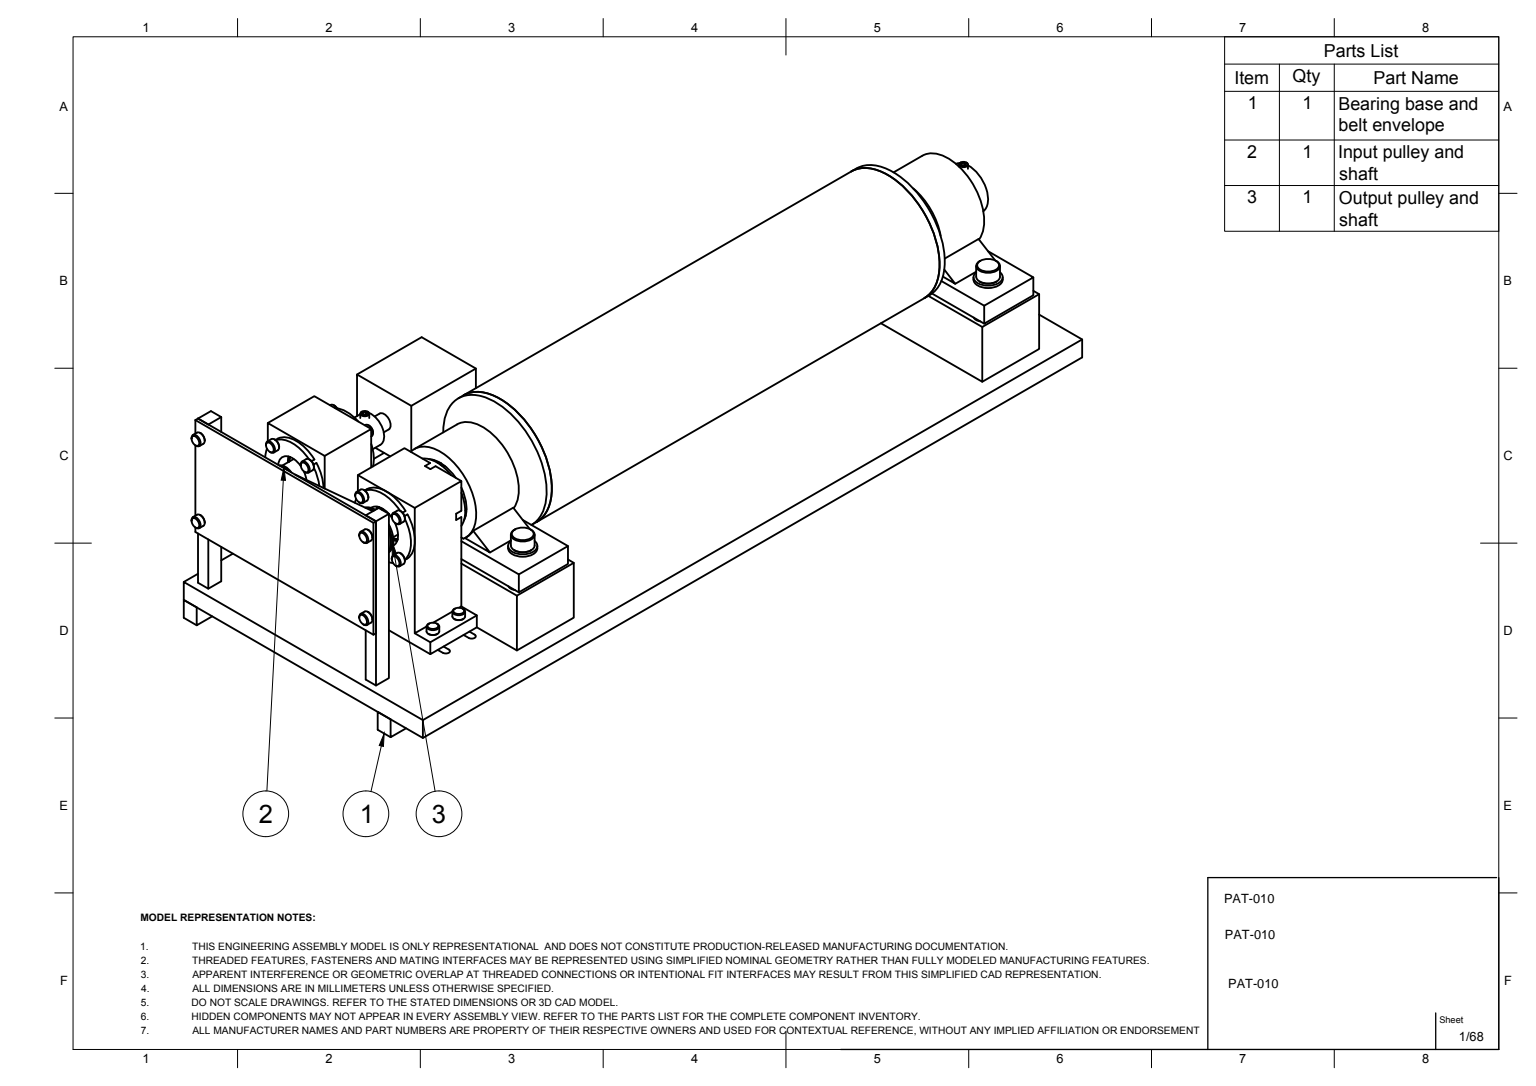
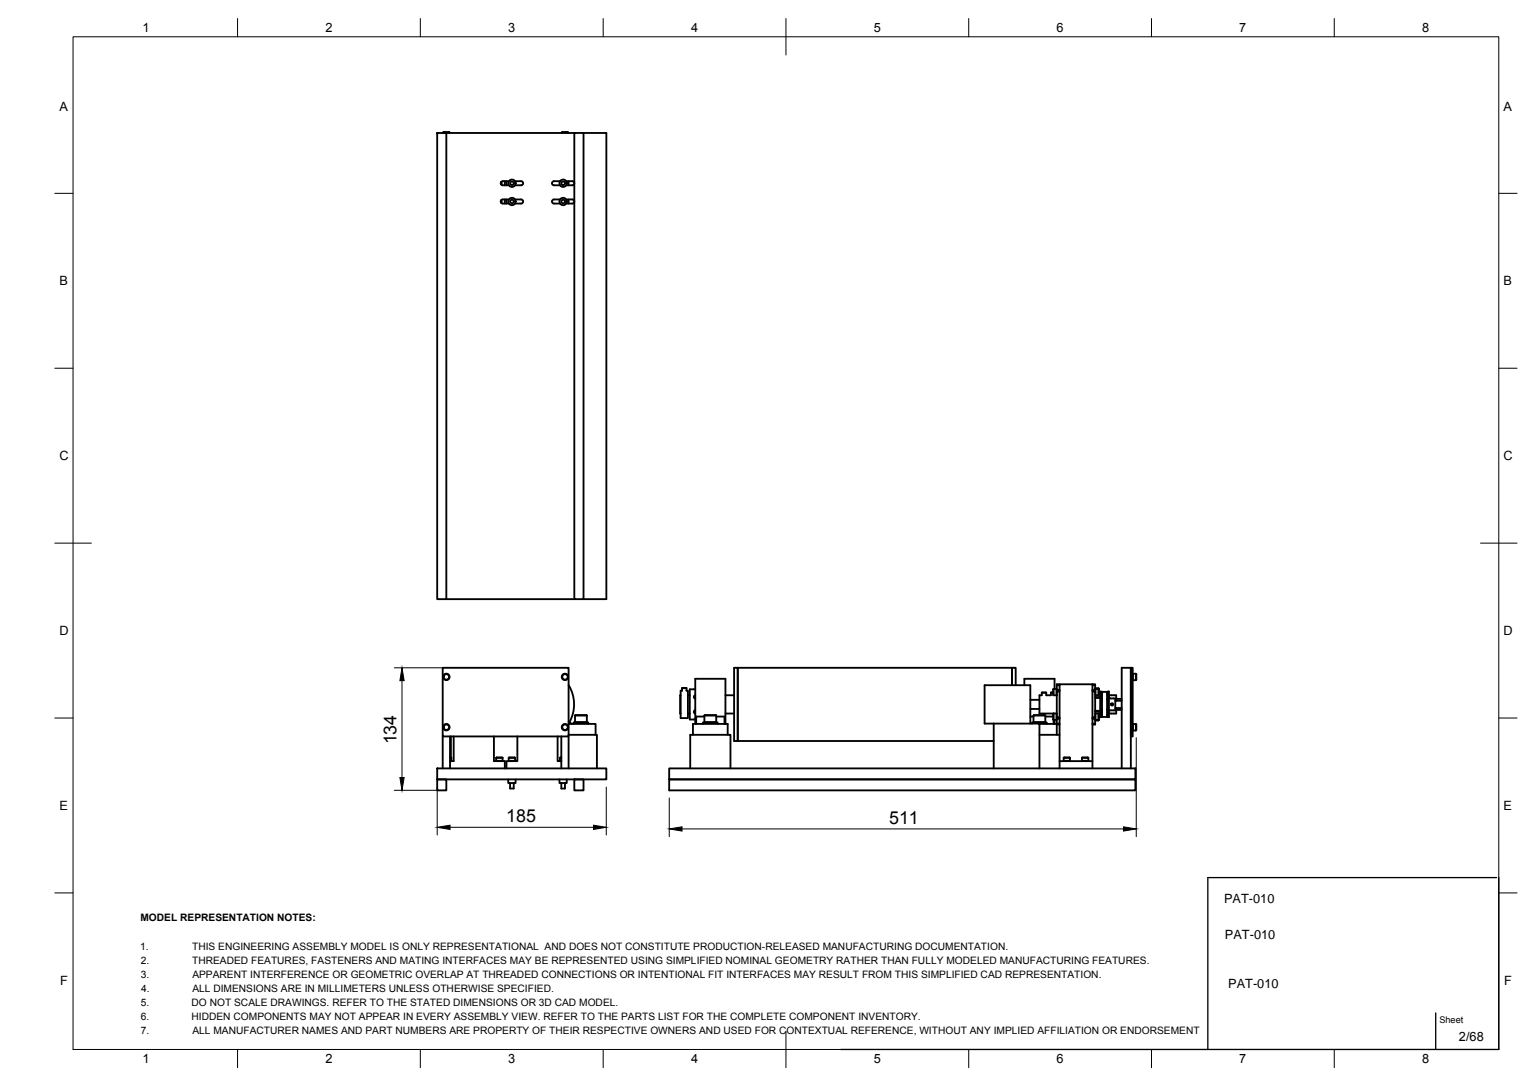
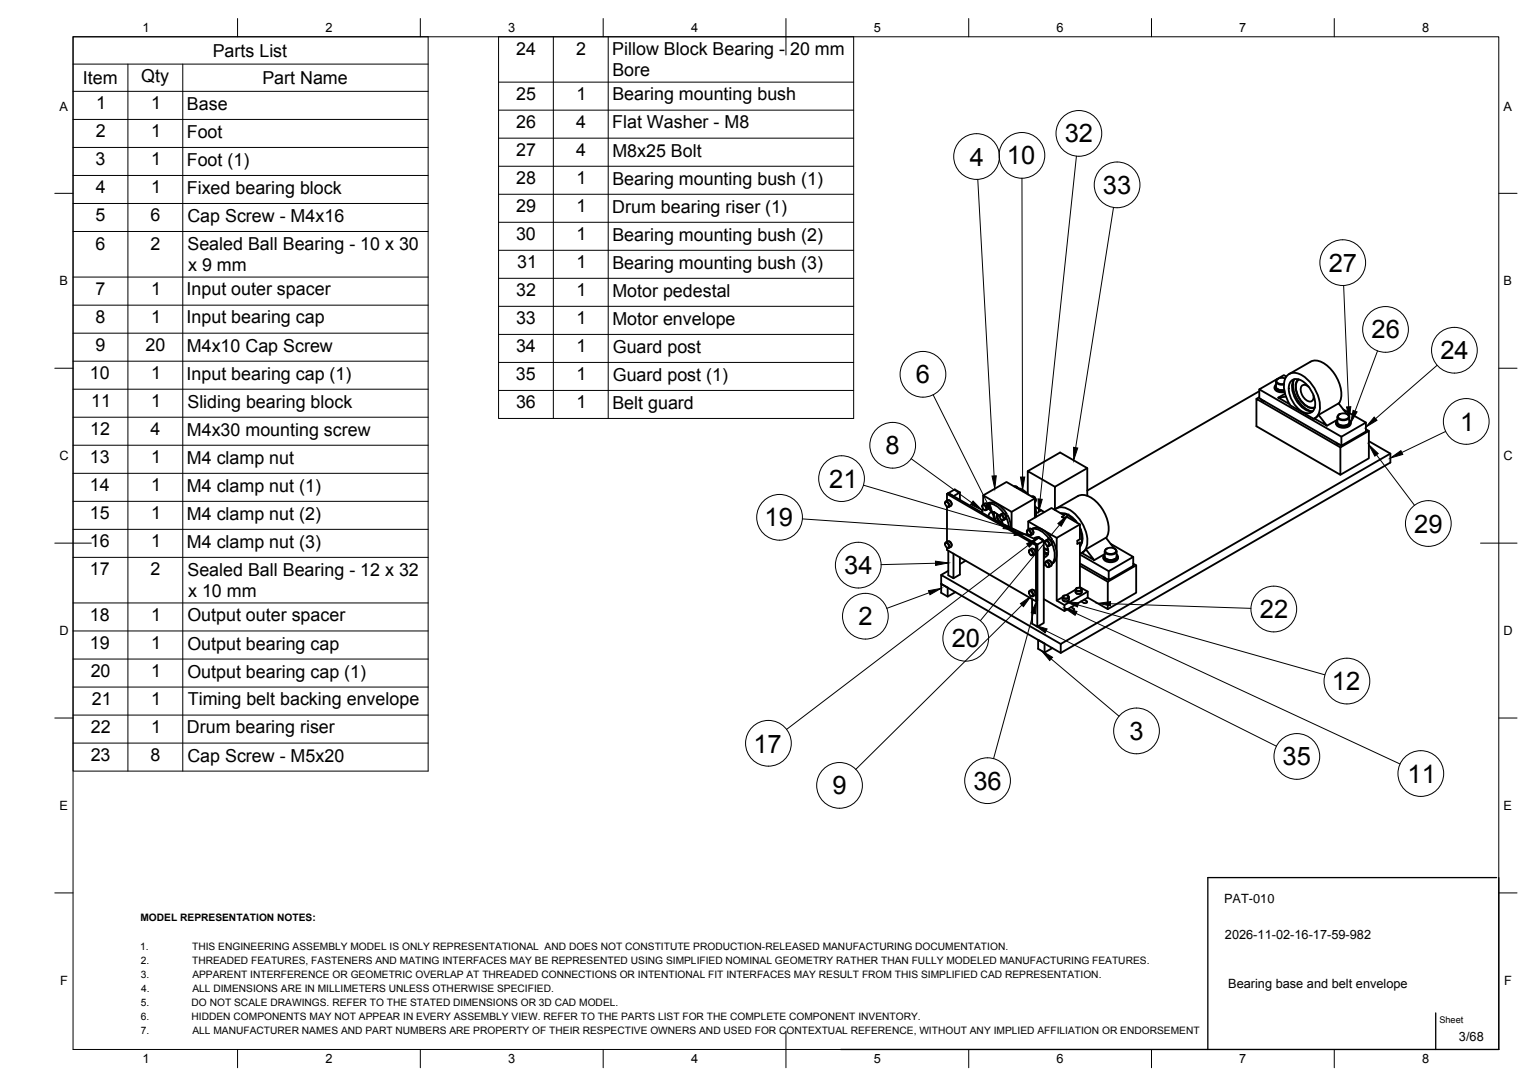
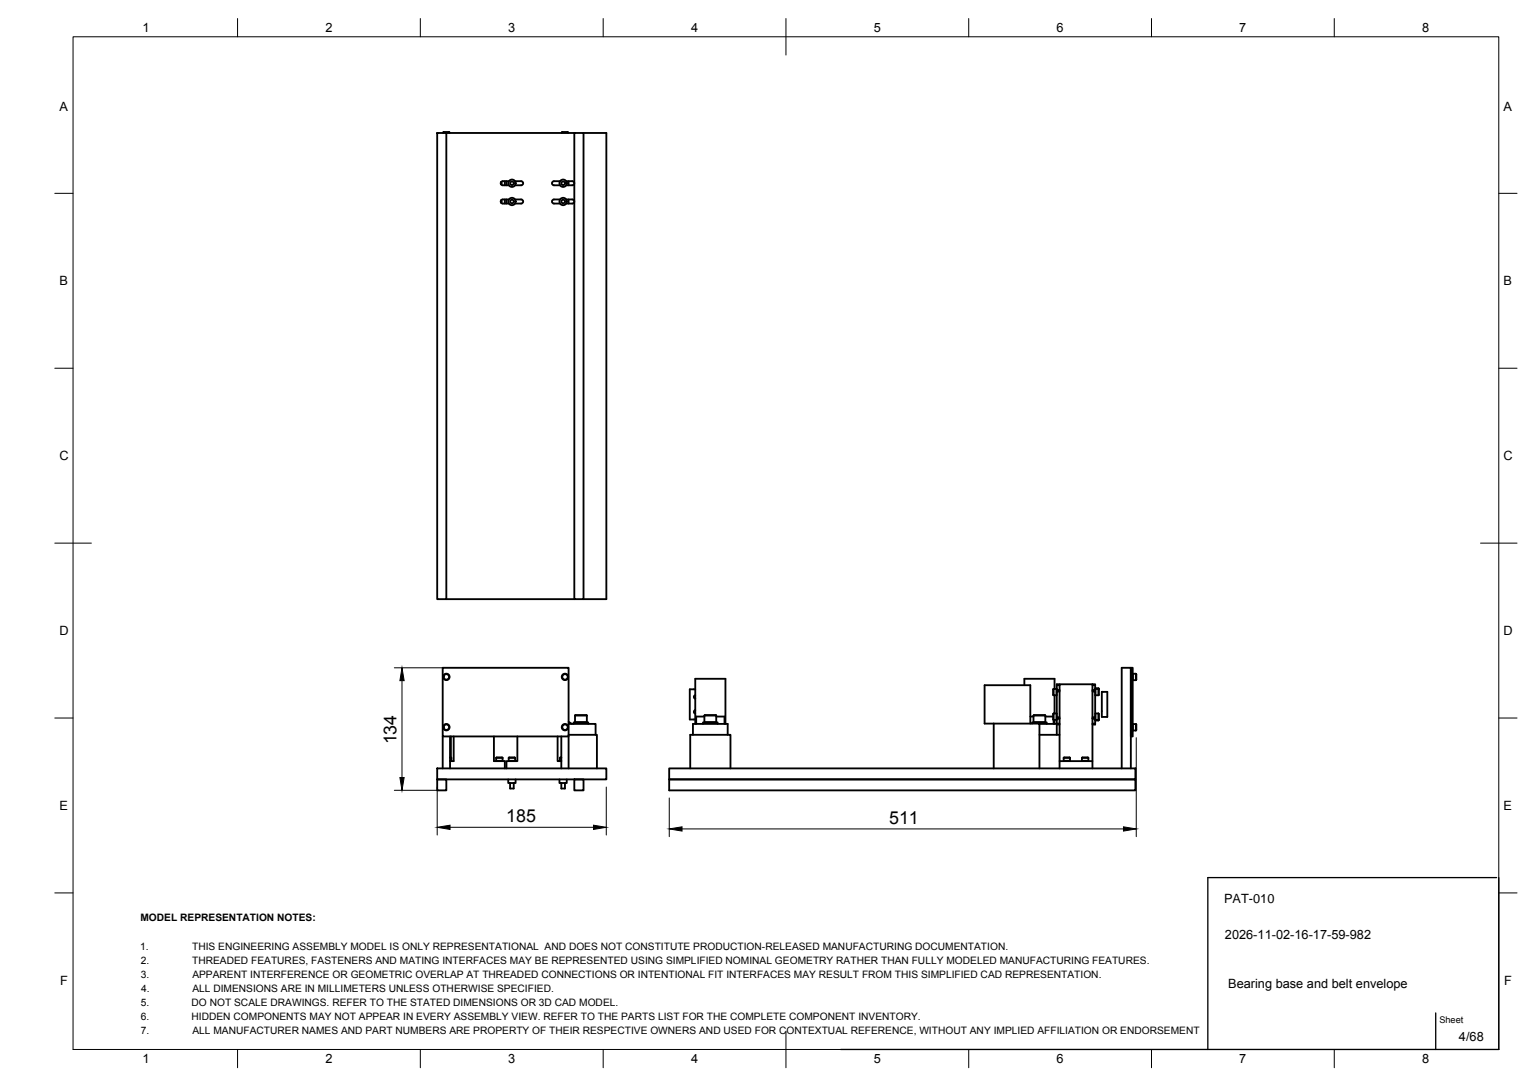
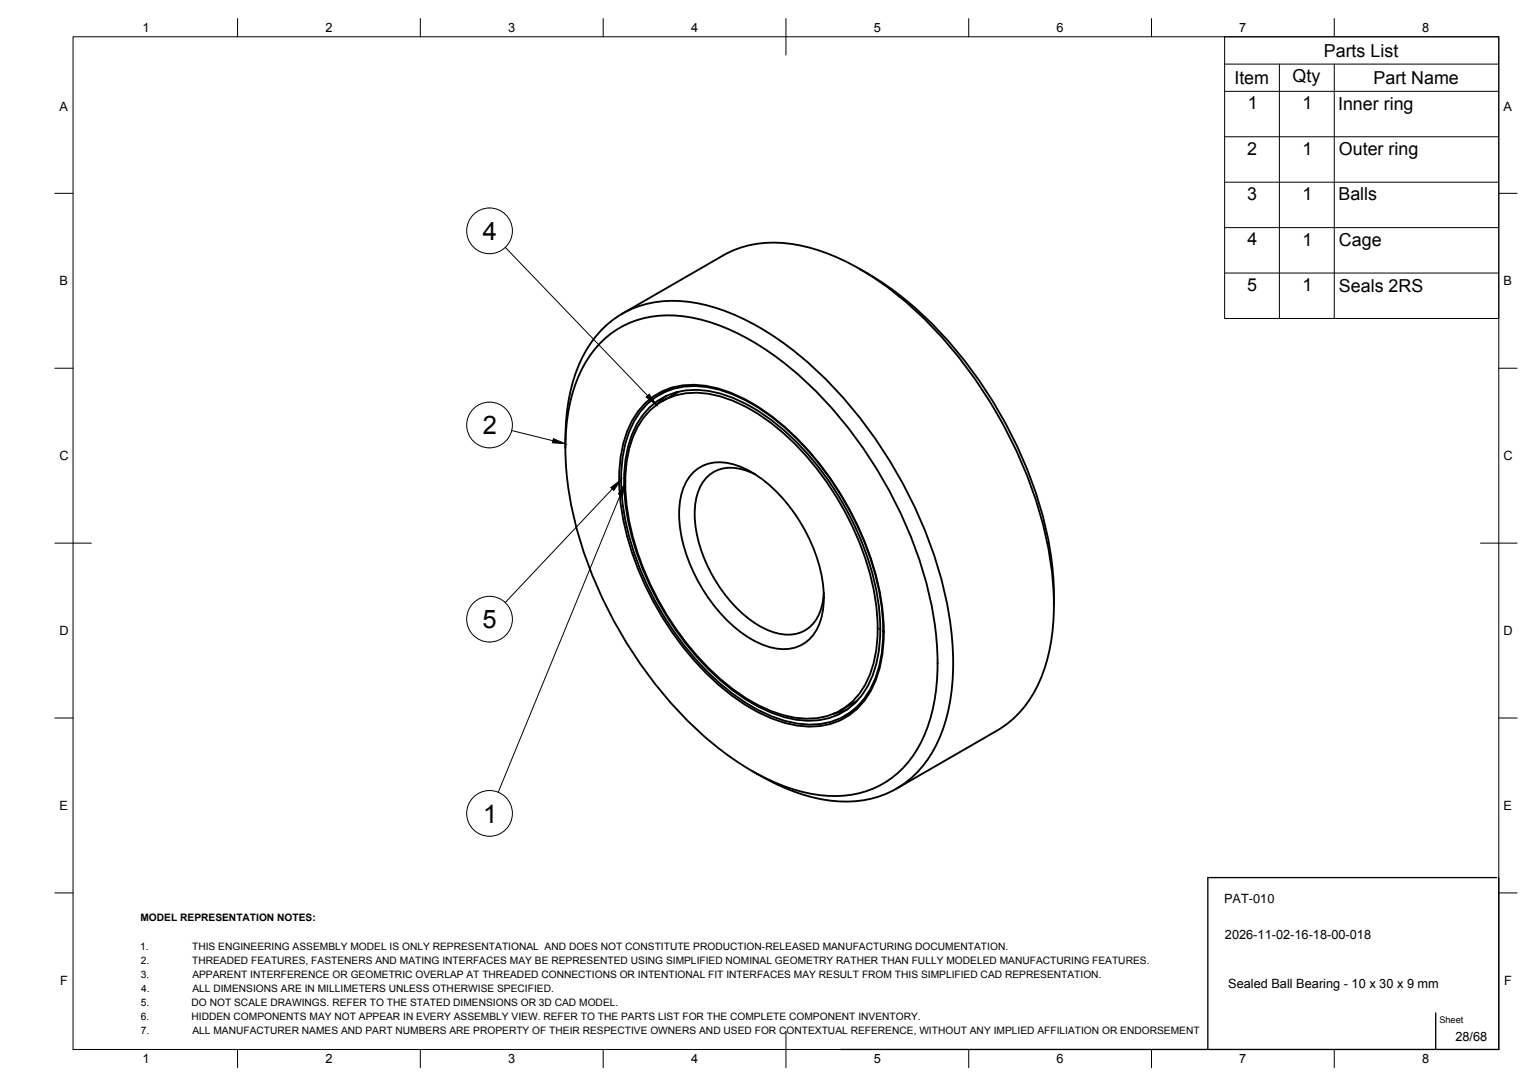
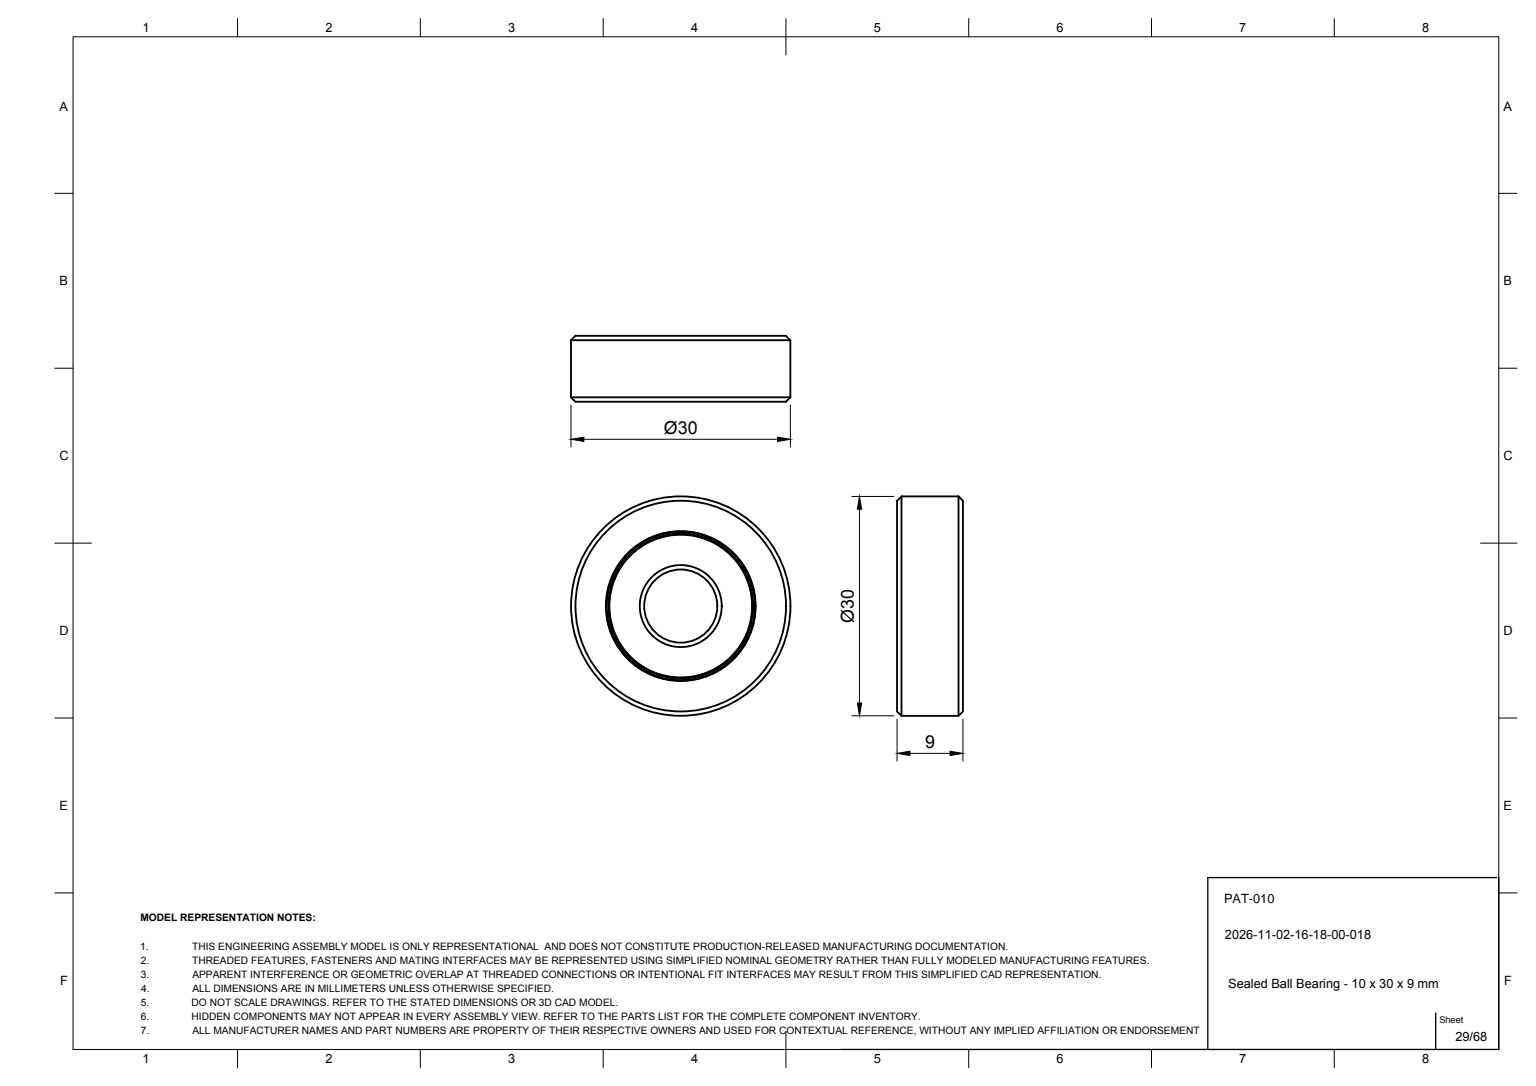
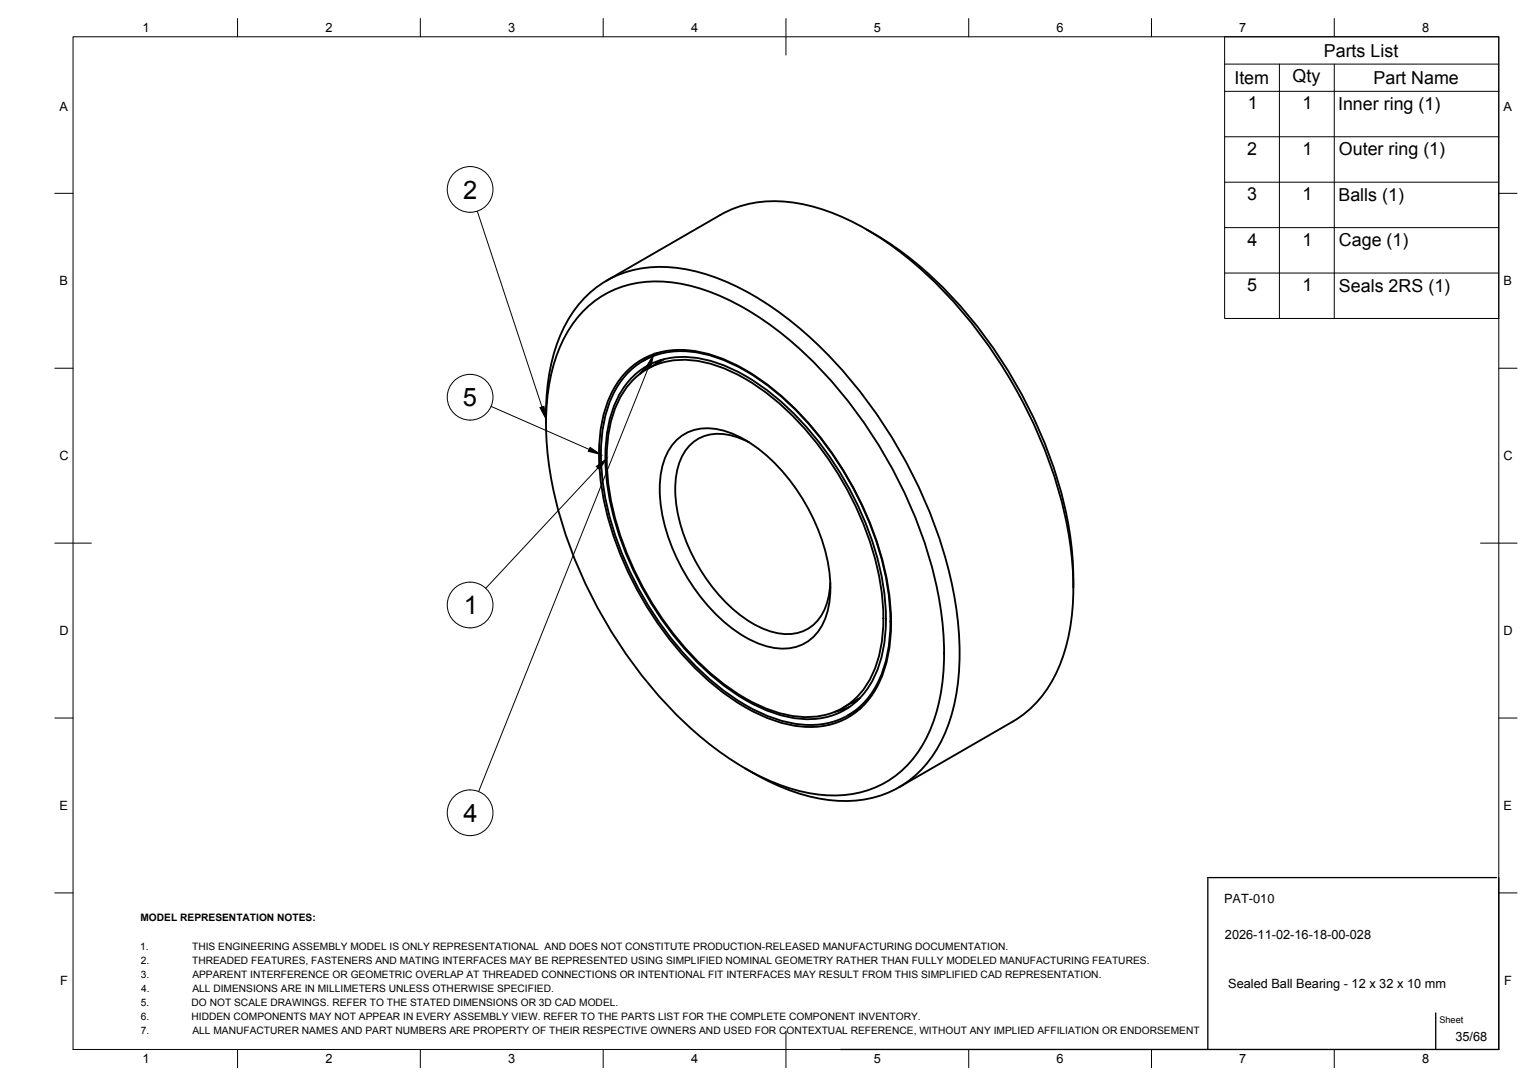
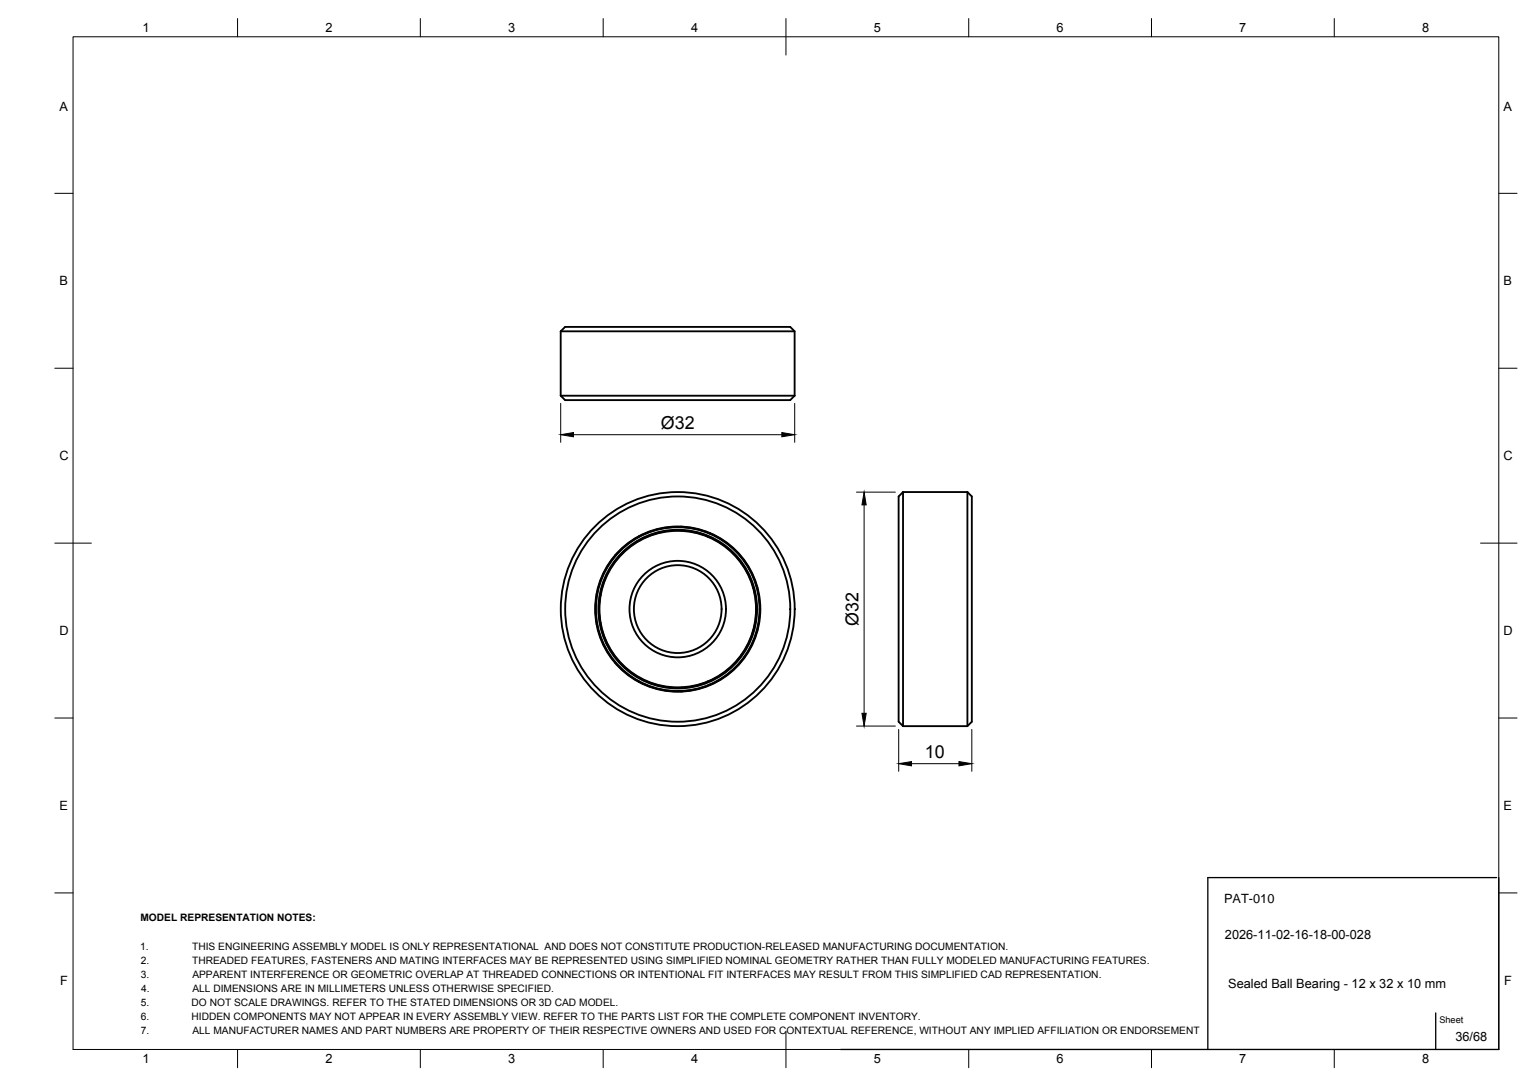
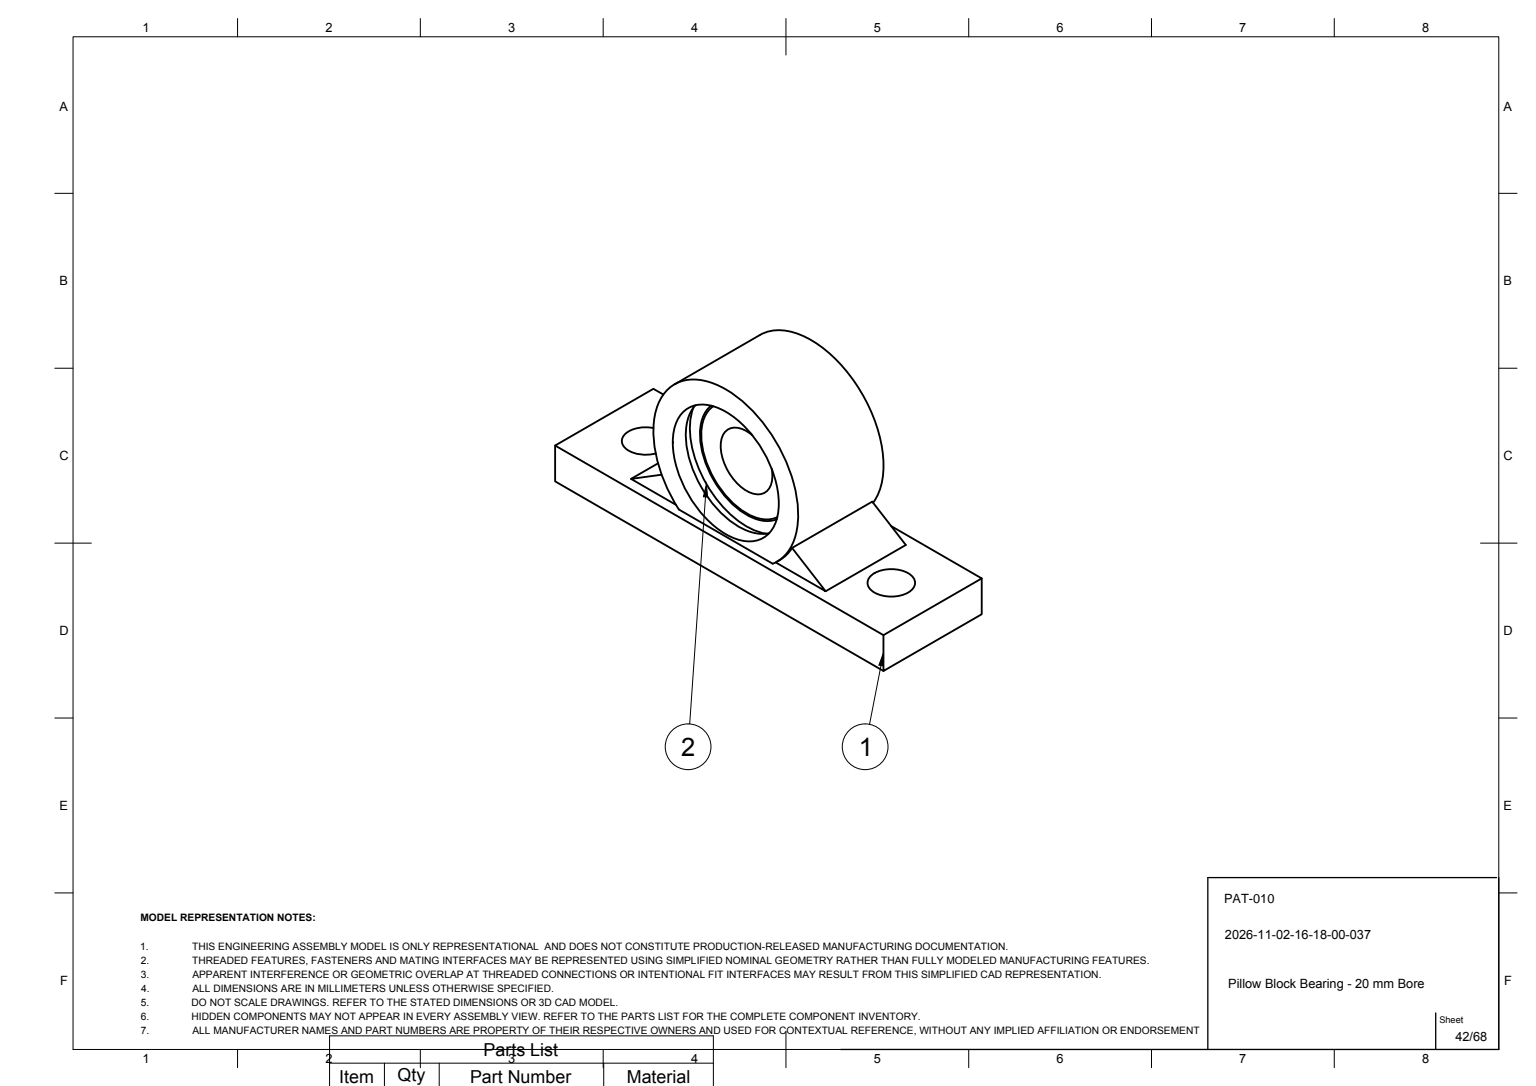
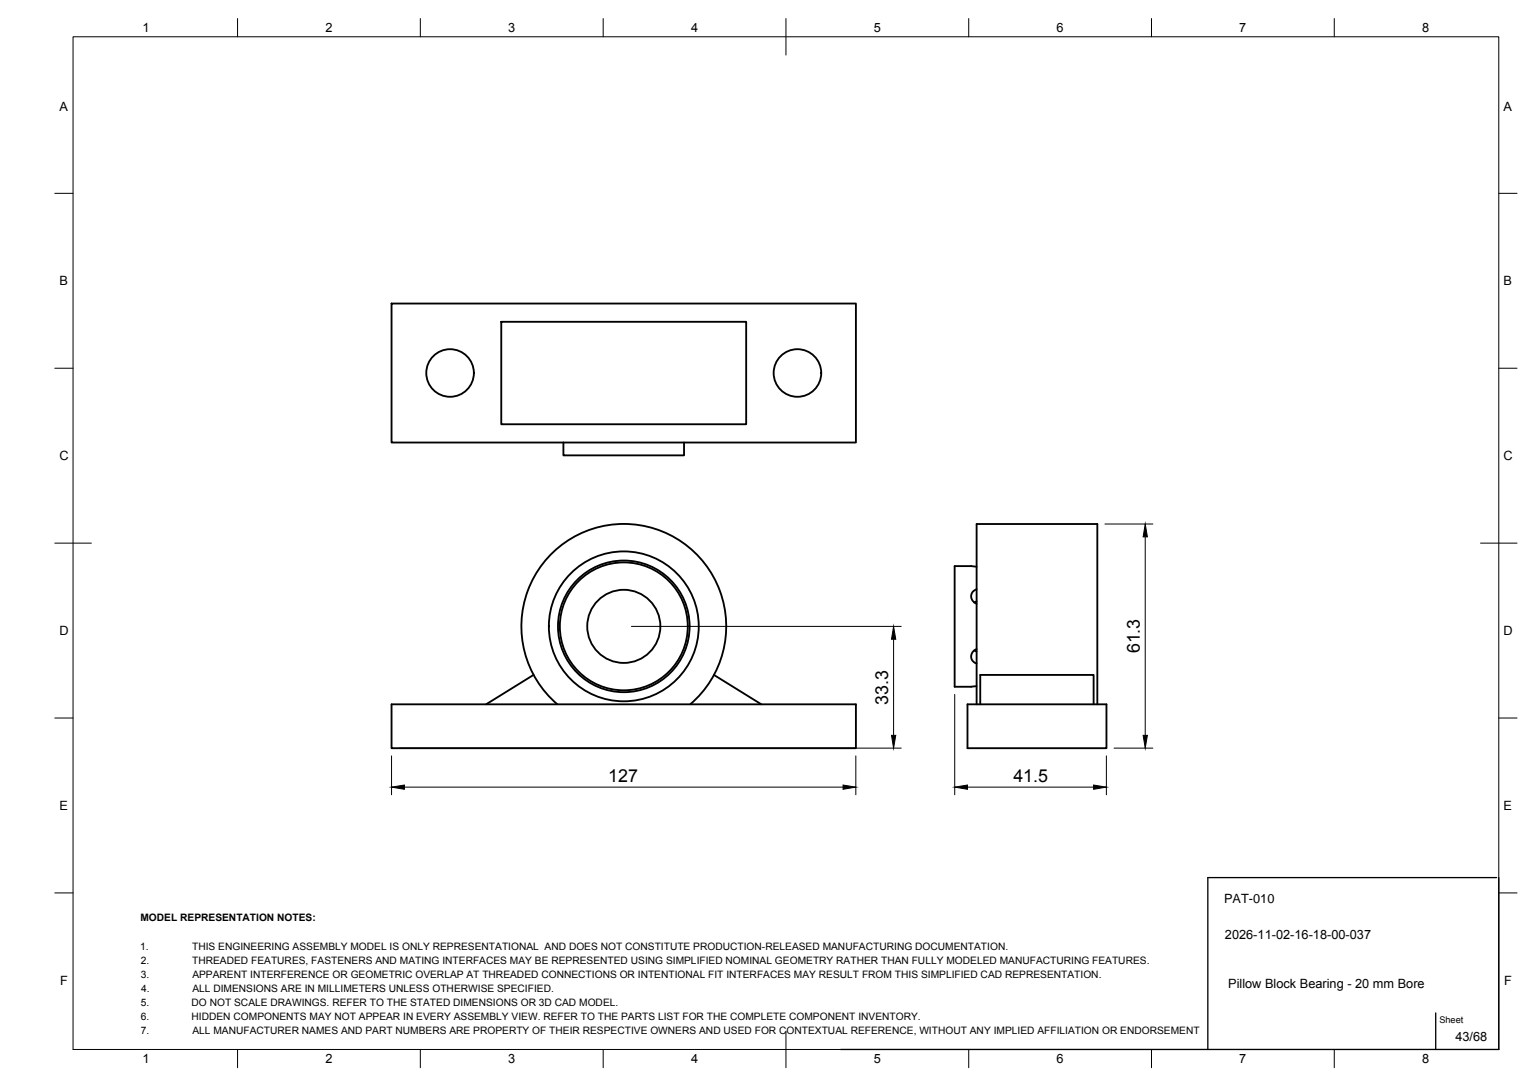
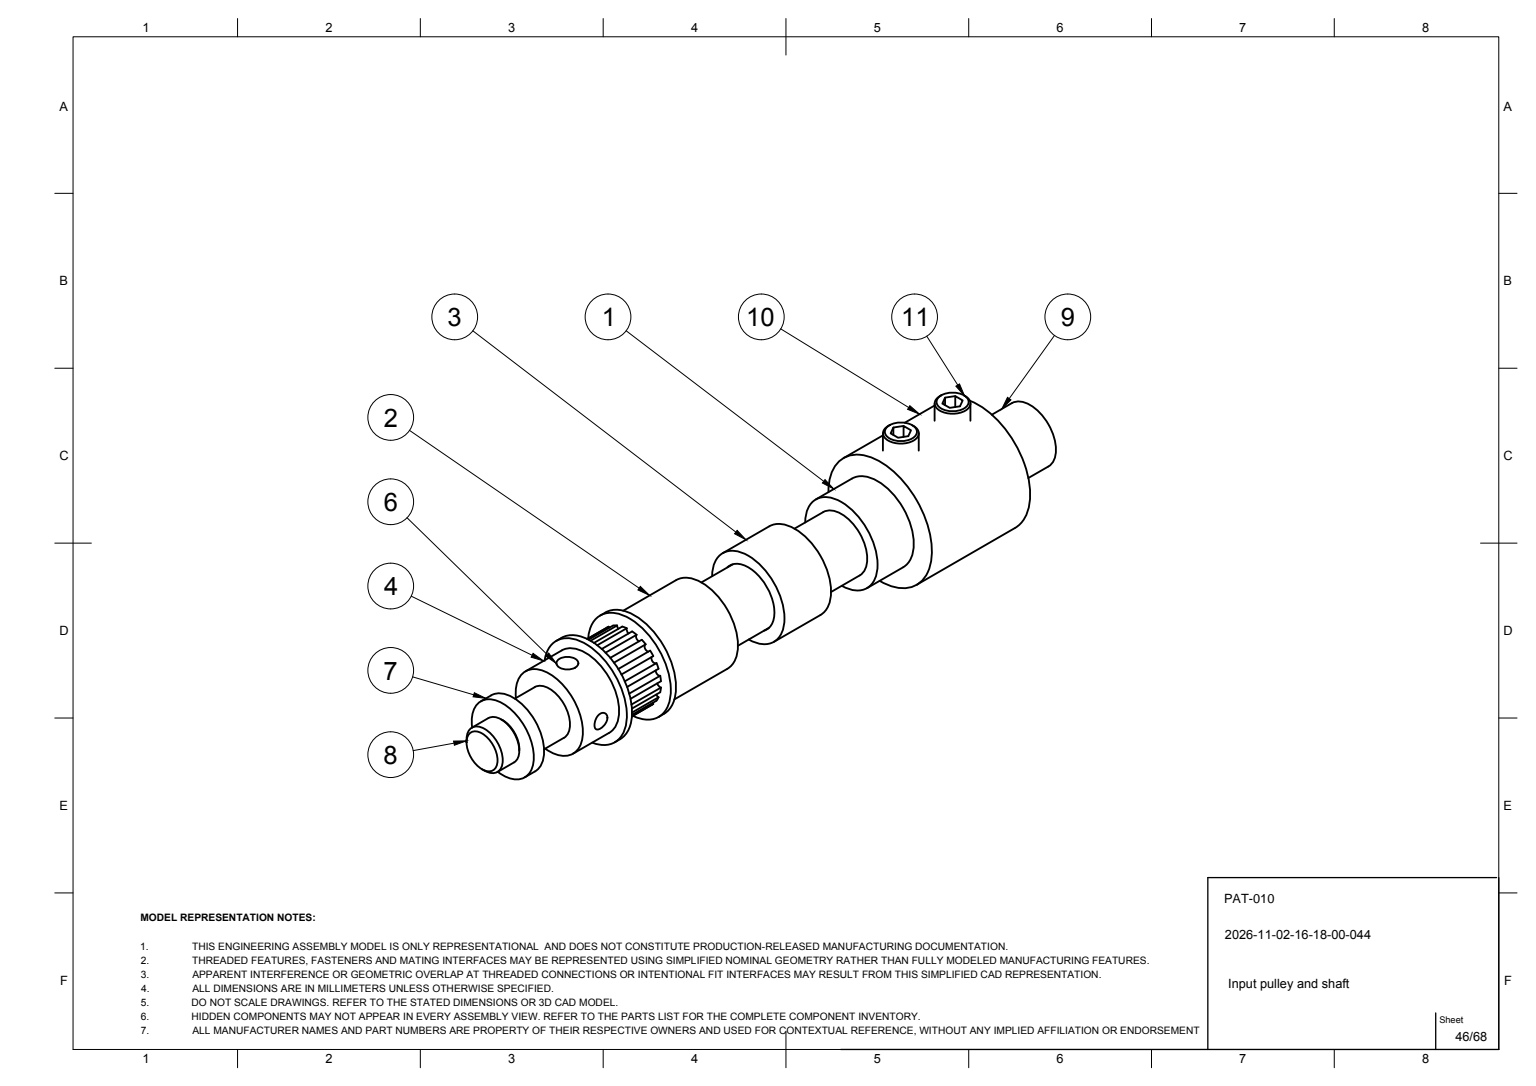
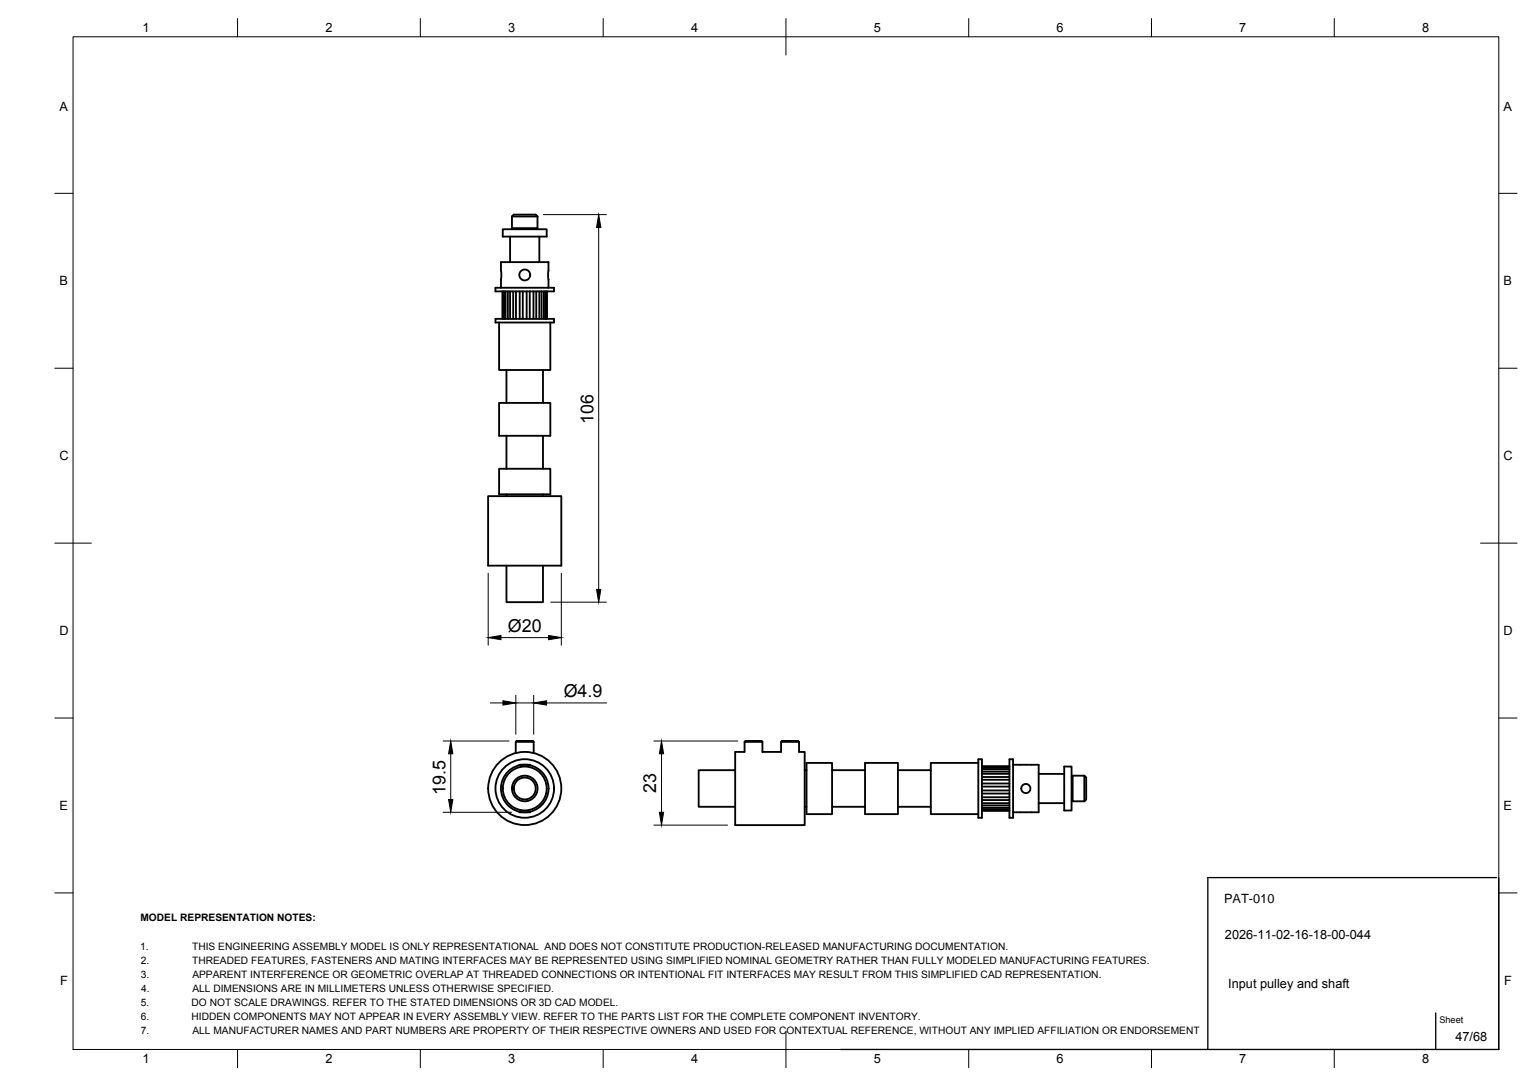
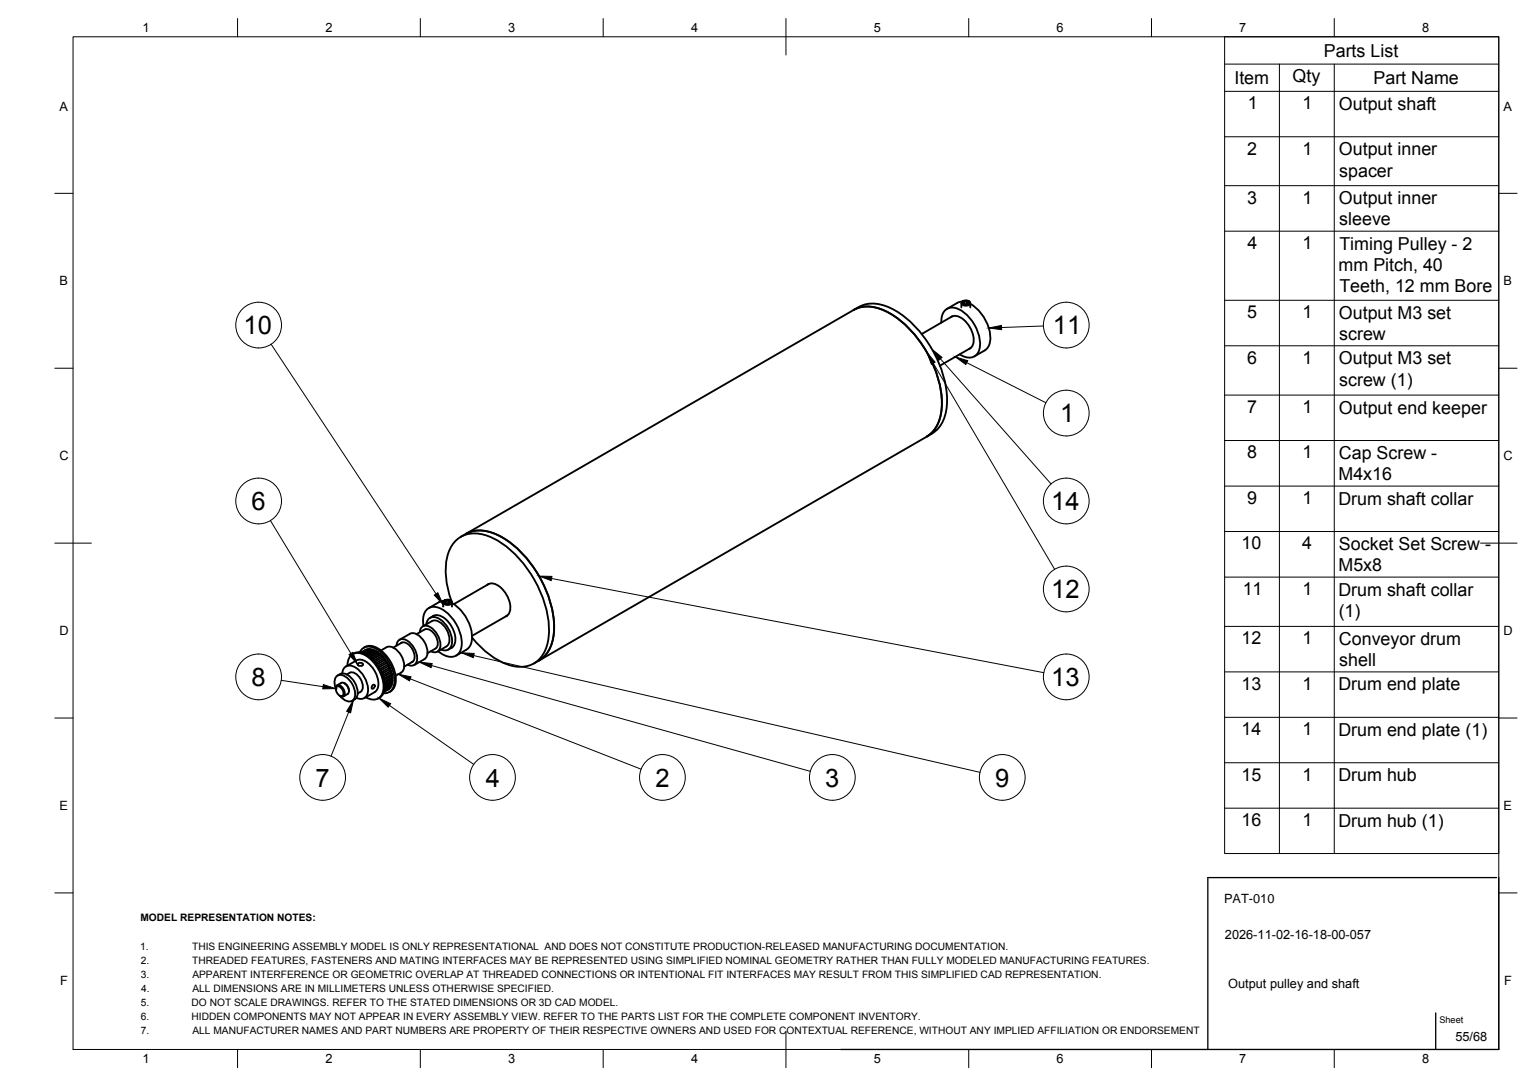
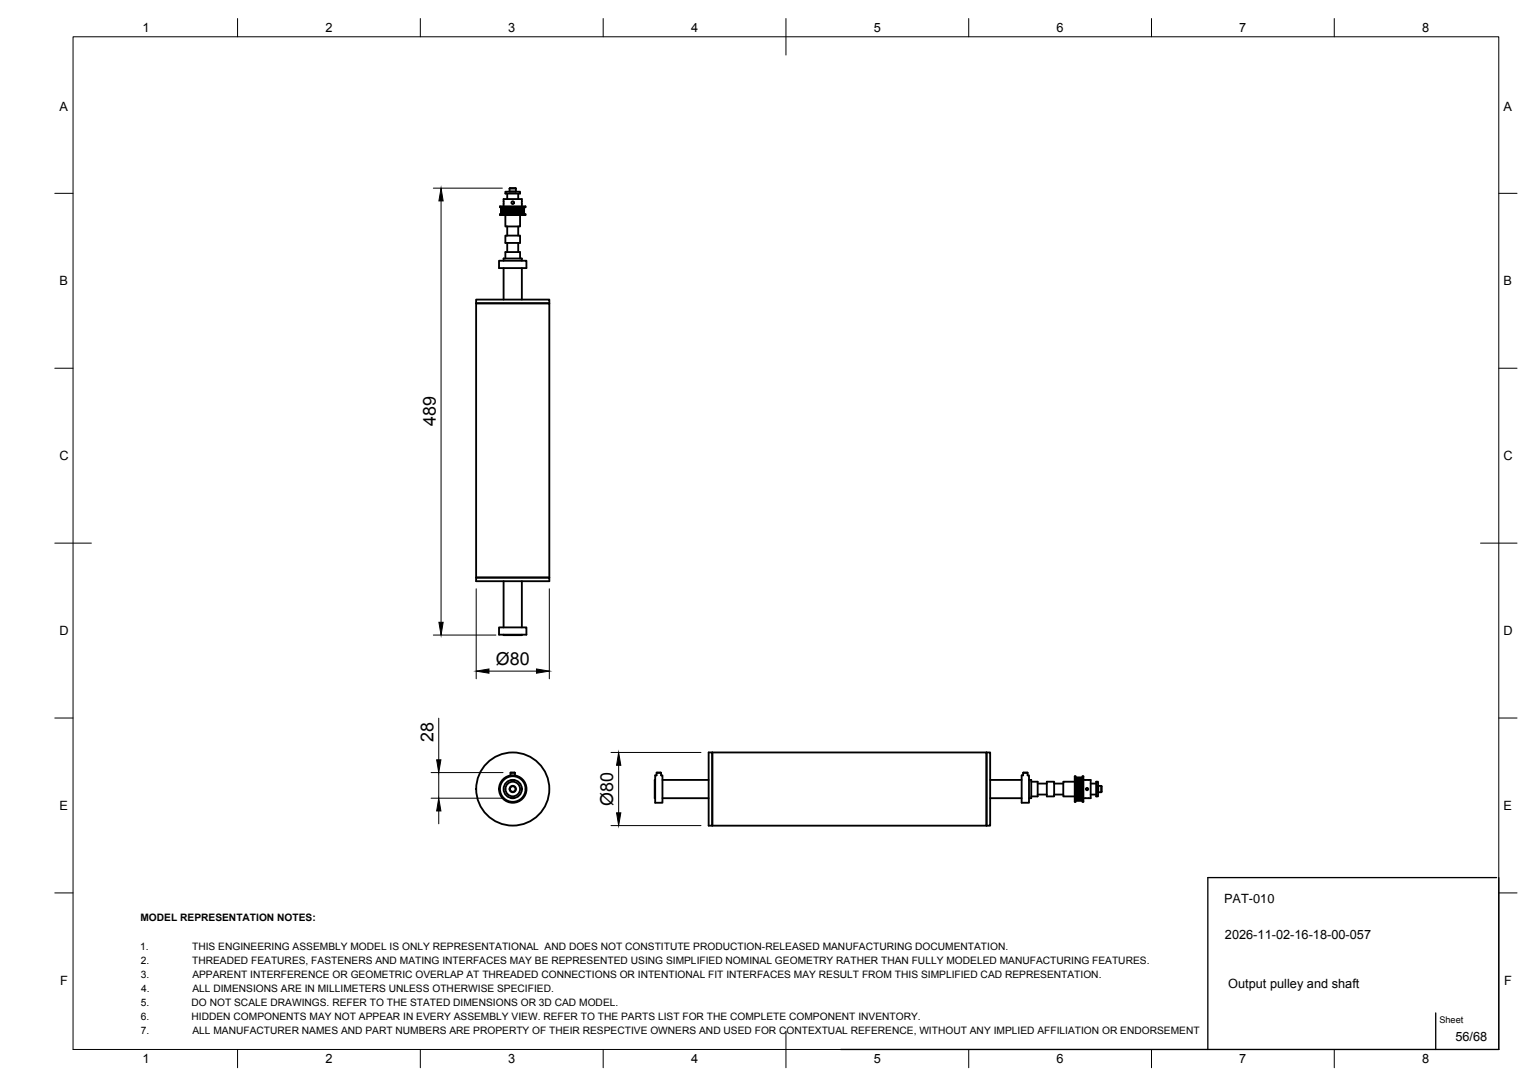
ISO-10303-21;
HEADER;
/* Generated by software containing ST-Developer
 * from STEP Tools, Inc. (www.steptools.com) 
 */

FILE_DESCRIPTION(
/* description */ ('Belt conveyor head drive unit'),
/* implementation_level */ '2;1');

FILE_NAME(
/* name */ 'PAT-010',
/* time_stamp */ '2026-10-28T03:26:19-07:00',
/* author */ (''),
/* organization */ (''),
/* preprocessor_version */ 'ST-DEVELOPER v20.2',
/* originating_system */ 'Autodesk Translation Framework v15.17.0.0',
/* authorisation */ '');

FILE_SCHEMA (('AUTOMOTIVE_DESIGN { 1 0 10303 214 3 1 1 }'));
ENDSEC;

DATA;
#10=MECHANICAL_DESIGN_GEOMETRIC_PRESENTATION_REPRESENTATION('',(#847,#848,
#849,#850,#851,#852,#853,#854,#855,#856,#857,#858,#859,#860,#861,#862,#863,
#864,#865,#866,#867,#868,#869,#870,#871,#872,#873,#874,#875,#876,#877,#878,
#879,#880,#881,#882,#883,#884,#885,#886,#887,#888,#889,#890,#891,#892,#893,
#894,#895,#896,#897,#898,#899,#900,#901,#902,#903,#904,#905,#906,#907,#908,
#909,#910,#911,#912,#913,#914,#915,#916,#917,#918,#919,#920,#921,#922,#923,
#924,#925,#926,#927,#928,#929,#930,#931),#27069);
#11=ORIENTED_CLOSED_SHELL('',*,#13752,.F.);
#12=ORIENTED_CLOSED_SHELL('',*,#13767,.F.);
#13=ORIENTED_CLOSED_SHELL('',*,#13772,.F.);
#14=ORIENTED_CLOSED_SHELL('',*,#13774,.F.);
#15=ORIENTED_CLOSED_SHELL('',*,#13800,.F.);
#16=BREP_WITH_VOIDS('Body1',#13753,(#11));
#17=BREP_WITH_VOIDS('Body1',#13766,(#12));
#18=BREP_WITH_VOIDS('Body1',#13773,(#13));
#19=BREP_WITH_VOIDS('Body1',#13775,(#14));
#20=BREP_WITH_VOIDS('Body1',#13799,(#15));
#21=ITEM_DEFINED_TRANSFORMATION($,$,#15190,#15318);
#22=ITEM_DEFINED_TRANSFORMATION($,$,#15210,#15319);
#23=ITEM_DEFINED_TRANSFORMATION($,$,#15230,#15320);
#24=ITEM_DEFINED_TRANSFORMATION($,$,#15247,#15321);
#25=ITEM_DEFINED_TRANSFORMATION($,$,#15301,#15322);
#26=ITEM_DEFINED_TRANSFORMATION($,$,#15354,#15476);
#27=ITEM_DEFINED_TRANSFORMATION($,$,#15374,#15477);
#28=ITEM_DEFINED_TRANSFORMATION($,$,#15394,#15478);
#29=ITEM_DEFINED_TRANSFORMATION($,$,#15409,#15479);
#30=ITEM_DEFINED_TRANSFORMATION($,$,#15459,#15480);
#31=ITEM_DEFINED_TRANSFORMATION($,$,#15508,#15577);
#32=ITEM_DEFINED_TRANSFORMATION($,$,#15549,#15578);
#33=ITEM_DEFINED_TRANSFORMATION($,$,#14564,#16304);
#34=ITEM_DEFINED_TRANSFORMATION($,$,#14663,#16305);
#35=ITEM_DEFINED_TRANSFORMATION($,$,#14670,#16306);
#36=ITEM_DEFINED_TRANSFORMATION($,$,#14677,#16307);
#37=ITEM_DEFINED_TRANSFORMATION($,$,#14715,#16308);
#38=ITEM_DEFINED_TRANSFORMATION($,$,#14724,#16309);
#39=ITEM_DEFINED_TRANSFORMATION($,$,#14758,#16310);
#40=ITEM_DEFINED_TRANSFORMATION($,$,#14792,#16311);
#41=ITEM_DEFINED_TRANSFORMATION($,$,#14842,#16312);
#42=ITEM_DEFINED_TRANSFORMATION($,$,#14851,#16313);
#43=ITEM_DEFINED_TRANSFORMATION($,$,#14860,#16314);
#44=ITEM_DEFINED_TRANSFORMATION($,$,#14869,#16315);
#45=ITEM_DEFINED_TRANSFORMATION($,$,#14878,#16316);
#46=ITEM_DEFINED_TRANSFORMATION($,$,#14887,#16317);
#47=ITEM_DEFINED_TRANSFORMATION($,$,#14921,#16318);
#48=ITEM_DEFINED_TRANSFORMATION($,$,#14975,#16319);
#49=ITEM_DEFINED_TRANSFORMATION($,$,#14994,#16320);
#50=ITEM_DEFINED_TRANSFORMATION($,$,#15037,#16321);
#51=ITEM_DEFINED_TRANSFORMATION($,$,#15046,#16322);
#52=ITEM_DEFINED_TRANSFORMATION($,$,#15055,#16323);
#53=ITEM_DEFINED_TRANSFORMATION($,$,#15098,#16324);
#54=ITEM_DEFINED_TRANSFORMATION($,$,#15107,#16325);
#55=ITEM_DEFINED_TRANSFORMATION($,$,#15116,#16326);
#56=ITEM_DEFINED_TRANSFORMATION($,$,#15137,#16327);
#57=ITEM_DEFINED_TRANSFORMATION($,$,#15144,#16328);
#58=ITEM_DEFINED_TRANSFORMATION($,$,#15157,#16329);
#59=ITEM_DEFINED_TRANSFORMATION($,$,#15170,#16330);
#60=ITEM_DEFINED_TRANSFORMATION($,$,#16278,#16331);
#61=ITEM_DEFINED_TRANSFORMATION($,$,#16278,#16332);
#62=ITEM_DEFINED_TRANSFORMATION($,$,#16278,#16333);
#63=ITEM_DEFINED_TRANSFORMATION($,$,#16278,#16334);
#64=ITEM_DEFINED_TRANSFORMATION($,$,#15189,#16335);
#65=ITEM_DEFINED_TRANSFORMATION($,$,#15189,#16336);
#66=ITEM_DEFINED_TRANSFORMATION($,$,#15612,#16337);
#67=ITEM_DEFINED_TRANSFORMATION($,$,#15612,#16338);
#68=ITEM_DEFINED_TRANSFORMATION($,$,#15612,#16339);
#69=ITEM_DEFINED_TRANSFORMATION($,$,#15612,#16340);
#70=ITEM_DEFINED_TRANSFORMATION($,$,#15612,#16341);
#71=ITEM_DEFINED_TRANSFORMATION($,$,#15612,#16342);
#72=ITEM_DEFINED_TRANSFORMATION($,$,#15612,#16343);
#73=ITEM_DEFINED_TRANSFORMATION($,$,#15612,#16344);
#74=ITEM_DEFINED_TRANSFORMATION($,$,#15323,#16345);
#75=ITEM_DEFINED_TRANSFORMATION($,$,#15323,#16346);
#76=ITEM_DEFINED_TRANSFORMATION($,$,#15323,#16347);
#77=ITEM_DEFINED_TRANSFORMATION($,$,#15323,#16348);
#78=ITEM_DEFINED_TRANSFORMATION($,$,#15353,#16349);
#79=ITEM_DEFINED_TRANSFORMATION($,$,#15353,#16350);
#80=ITEM_DEFINED_TRANSFORMATION($,$,#15612,#16351);
#81=ITEM_DEFINED_TRANSFORMATION($,$,#15612,#16352);
#82=ITEM_DEFINED_TRANSFORMATION($,$,#15612,#16353);
#83=ITEM_DEFINED_TRANSFORMATION($,$,#15612,#16354);
#84=ITEM_DEFINED_TRANSFORMATION($,$,#15612,#16355);
#85=ITEM_DEFINED_TRANSFORMATION($,$,#15612,#16356);
#86=ITEM_DEFINED_TRANSFORMATION($,$,#15612,#16357);
#87=ITEM_DEFINED_TRANSFORMATION($,$,#15612,#16358);
#88=ITEM_DEFINED_TRANSFORMATION($,$,#15481,#16359);
#89=ITEM_DEFINED_TRANSFORMATION($,$,#15481,#16360);
#90=ITEM_DEFINED_TRANSFORMATION($,$,#15481,#16361);
#91=ITEM_DEFINED_TRANSFORMATION($,$,#15481,#16362);
#92=ITEM_DEFINED_TRANSFORMATION($,$,#15507,#16363);
#93=ITEM_DEFINED_TRANSFORMATION($,$,#15579,#16364);
#94=ITEM_DEFINED_TRANSFORMATION($,$,#15588,#16365);
#95=ITEM_DEFINED_TRANSFORMATION($,$,#15579,#16366);
#96=ITEM_DEFINED_TRANSFORMATION($,$,#15588,#16367);
#97=ITEM_DEFINED_TRANSFORMATION($,$,#15481,#16368);
#98=ITEM_DEFINED_TRANSFORMATION($,$,#15481,#16369);
#99=ITEM_DEFINED_TRANSFORMATION($,$,#15481,#16370);
#100=ITEM_DEFINED_TRANSFORMATION($,$,#15481,#16371);
#101=ITEM_DEFINED_TRANSFORMATION($,$,#15507,#16372);
#102=ITEM_DEFINED_TRANSFORMATION($,$,#15579,#16373);
#103=ITEM_DEFINED_TRANSFORMATION($,$,#15588,#16374);
#104=ITEM_DEFINED_TRANSFORMATION($,$,#15579,#16375);
#105=ITEM_DEFINED_TRANSFORMATION($,$,#15588,#16376);
#106=ITEM_DEFINED_TRANSFORMATION($,$,#16278,#16377);
#107=ITEM_DEFINED_TRANSFORMATION($,$,#16278,#16378);
#108=ITEM_DEFINED_TRANSFORMATION($,$,#15612,#16379);
#109=ITEM_DEFINED_TRANSFORMATION($,$,#15612,#16380);
#110=ITEM_DEFINED_TRANSFORMATION($,$,#15612,#16381);
#111=ITEM_DEFINED_TRANSFORMATION($,$,#15612,#16382);
#112=ITEM_DEFINED_TRANSFORMATION($,$,#15637,#16400);
#113=ITEM_DEFINED_TRANSFORMATION($,$,#15659,#16401);
#114=ITEM_DEFINED_TRANSFORMATION($,$,#15672,#16402);
#115=ITEM_DEFINED_TRANSFORMATION($,$,#15681,#16403);
#116=ITEM_DEFINED_TRANSFORMATION($,$,#15687,#16404);
#117=ITEM_DEFINED_TRANSFORMATION($,$,#15693,#16405);
#118=ITEM_DEFINED_TRANSFORMATION($,$,#15702,#16406);
#119=ITEM_DEFINED_TRANSFORMATION($,$,#15708,#16407);
#120=ITEM_DEFINED_TRANSFORMATION($,$,#15729,#16408);
#121=ITEM_DEFINED_TRANSFORMATION($,$,#16278,#16409);
#122=ITEM_DEFINED_TRANSFORMATION($,$,#16383,#16410);
#123=ITEM_DEFINED_TRANSFORMATION($,$,#16383,#16411);
#124=ITEM_DEFINED_TRANSFORMATION($,$,#15872,#16412);
#125=ITEM_DEFINED_TRANSFORMATION($,$,#15890,#16413);
#126=ITEM_DEFINED_TRANSFORMATION($,$,#15899,#16414);
#127=ITEM_DEFINED_TRANSFORMATION($,$,#15908,#16415);
#128=ITEM_DEFINED_TRANSFORMATION($,$,#15914,#16416);
#129=ITEM_DEFINED_TRANSFORMATION($,$,#15920,#16417);
#130=ITEM_DEFINED_TRANSFORMATION($,$,#15929,#16418);
#131=ITEM_DEFINED_TRANSFORMATION($,$,#15944,#16419);
#132=ITEM_DEFINED_TRANSFORMATION($,$,#15959,#16420);
#133=ITEM_DEFINED_TRANSFORMATION($,$,#15968,#16421);
#134=ITEM_DEFINED_TRANSFORMATION($,$,#15977,#16422);
#135=ITEM_DEFINED_TRANSFORMATION($,$,#15986,#16423);
#136=ITEM_DEFINED_TRANSFORMATION($,$,#16001,#16424);
#137=ITEM_DEFINED_TRANSFORMATION($,$,#16016,#16425);
#138=ITEM_DEFINED_TRANSFORMATION($,$,#16278,#16426);
#139=ITEM_DEFINED_TRANSFORMATION($,$,#16383,#16427);
#140=ITEM_DEFINED_TRANSFORMATION($,$,#16383,#16428);
#141=ITEM_DEFINED_TRANSFORMATION($,$,#16383,#16429);
#142=ITEM_DEFINED_TRANSFORMATION($,$,#16383,#16430);
#143=ITEM_DEFINED_TRANSFORMATION($,$,#14563,#16431);
#144=ITEM_DEFINED_TRANSFORMATION($,$,#15636,#16432);
#145=ITEM_DEFINED_TRANSFORMATION($,$,#15871,#16433);
#146=(
REPRESENTATION_RELATIONSHIP($,$,#27381,#27380)
REPRESENTATION_RELATIONSHIP_WITH_TRANSFORMATION(#21)
SHAPE_REPRESENTATION_RELATIONSHIP()
);
#147=(
REPRESENTATION_RELATIONSHIP($,$,#27382,#27380)
REPRESENTATION_RELATIONSHIP_WITH_TRANSFORMATION(#22)
SHAPE_REPRESENTATION_RELATIONSHIP()
);
#148=(
REPRESENTATION_RELATIONSHIP($,$,#27383,#27380)
REPRESENTATION_RELATIONSHIP_WITH_TRANSFORMATION(#23)
SHAPE_REPRESENTATION_RELATIONSHIP()
);
#149=(
REPRESENTATION_RELATIONSHIP($,$,#27384,#27380)
REPRESENTATION_RELATIONSHIP_WITH_TRANSFORMATION(#24)
SHAPE_REPRESENTATION_RELATIONSHIP()
);
#150=(
REPRESENTATION_RELATIONSHIP($,$,#27385,#27380)
REPRESENTATION_RELATIONSHIP_WITH_TRANSFORMATION(#25)
SHAPE_REPRESENTATION_RELATIONSHIP()
);
#151=(
REPRESENTATION_RELATIONSHIP($,$,#27388,#27387)
REPRESENTATION_RELATIONSHIP_WITH_TRANSFORMATION(#26)
SHAPE_REPRESENTATION_RELATIONSHIP()
);
#152=(
REPRESENTATION_RELATIONSHIP($,$,#27389,#27387)
REPRESENTATION_RELATIONSHIP_WITH_TRANSFORMATION(#27)
SHAPE_REPRESENTATION_RELATIONSHIP()
);
#153=(
REPRESENTATION_RELATIONSHIP($,$,#27390,#27387)
REPRESENTATION_RELATIONSHIP_WITH_TRANSFORMATION(#28)
SHAPE_REPRESENTATION_RELATIONSHIP()
);
#154=(
REPRESENTATION_RELATIONSHIP($,$,#27391,#27387)
REPRESENTATION_RELATIONSHIP_WITH_TRANSFORMATION(#29)
SHAPE_REPRESENTATION_RELATIONSHIP()
);
#155=(
REPRESENTATION_RELATIONSHIP($,$,#27392,#27387)
REPRESENTATION_RELATIONSHIP_WITH_TRANSFORMATION(#30)
SHAPE_REPRESENTATION_RELATIONSHIP()
);
#156=(
REPRESENTATION_RELATIONSHIP($,$,#27395,#27394)
REPRESENTATION_RELATIONSHIP_WITH_TRANSFORMATION(#31)
SHAPE_REPRESENTATION_RELATIONSHIP()
);
#157=(
REPRESENTATION_RELATIONSHIP($,$,#27396,#27394)
REPRESENTATION_RELATIONSHIP_WITH_TRANSFORMATION(#32)
SHAPE_REPRESENTATION_RELATIONSHIP()
);
#158=(
REPRESENTATION_RELATIONSHIP($,$,#27353,#27352)
REPRESENTATION_RELATIONSHIP_WITH_TRANSFORMATION(#33)
SHAPE_REPRESENTATION_RELATIONSHIP()
);
#159=(
REPRESENTATION_RELATIONSHIP($,$,#27354,#27352)
REPRESENTATION_RELATIONSHIP_WITH_TRANSFORMATION(#34)
SHAPE_REPRESENTATION_RELATIONSHIP()
);
#160=(
REPRESENTATION_RELATIONSHIP($,$,#27355,#27352)
REPRESENTATION_RELATIONSHIP_WITH_TRANSFORMATION(#35)
SHAPE_REPRESENTATION_RELATIONSHIP()
);
#161=(
REPRESENTATION_RELATIONSHIP($,$,#27356,#27352)
REPRESENTATION_RELATIONSHIP_WITH_TRANSFORMATION(#36)
SHAPE_REPRESENTATION_RELATIONSHIP()
);
#162=(
REPRESENTATION_RELATIONSHIP($,$,#27357,#27352)
REPRESENTATION_RELATIONSHIP_WITH_TRANSFORMATION(#37)
SHAPE_REPRESENTATION_RELATIONSHIP()
);
#163=(
REPRESENTATION_RELATIONSHIP($,$,#27358,#27352)
REPRESENTATION_RELATIONSHIP_WITH_TRANSFORMATION(#38)
SHAPE_REPRESENTATION_RELATIONSHIP()
);
#164=(
REPRESENTATION_RELATIONSHIP($,$,#27359,#27352)
REPRESENTATION_RELATIONSHIP_WITH_TRANSFORMATION(#39)
SHAPE_REPRESENTATION_RELATIONSHIP()
);
#165=(
REPRESENTATION_RELATIONSHIP($,$,#27360,#27352)
REPRESENTATION_RELATIONSHIP_WITH_TRANSFORMATION(#40)
SHAPE_REPRESENTATION_RELATIONSHIP()
);
#166=(
REPRESENTATION_RELATIONSHIP($,$,#27361,#27352)
REPRESENTATION_RELATIONSHIP_WITH_TRANSFORMATION(#41)
SHAPE_REPRESENTATION_RELATIONSHIP()
);
#167=(
REPRESENTATION_RELATIONSHIP($,$,#27362,#27352)
REPRESENTATION_RELATIONSHIP_WITH_TRANSFORMATION(#42)
SHAPE_REPRESENTATION_RELATIONSHIP()
);
#168=(
REPRESENTATION_RELATIONSHIP($,$,#27363,#27352)
REPRESENTATION_RELATIONSHIP_WITH_TRANSFORMATION(#43)
SHAPE_REPRESENTATION_RELATIONSHIP()
);
#169=(
REPRESENTATION_RELATIONSHIP($,$,#27364,#27352)
REPRESENTATION_RELATIONSHIP_WITH_TRANSFORMATION(#44)
SHAPE_REPRESENTATION_RELATIONSHIP()
);
#170=(
REPRESENTATION_RELATIONSHIP($,$,#27365,#27352)
REPRESENTATION_RELATIONSHIP_WITH_TRANSFORMATION(#45)
SHAPE_REPRESENTATION_RELATIONSHIP()
);
#171=(
REPRESENTATION_RELATIONSHIP($,$,#27366,#27352)
REPRESENTATION_RELATIONSHIP_WITH_TRANSFORMATION(#46)
SHAPE_REPRESENTATION_RELATIONSHIP()
);
#172=(
REPRESENTATION_RELATIONSHIP($,$,#27367,#27352)
REPRESENTATION_RELATIONSHIP_WITH_TRANSFORMATION(#47)
SHAPE_REPRESENTATION_RELATIONSHIP()
);
#173=(
REPRESENTATION_RELATIONSHIP($,$,#27368,#27352)
REPRESENTATION_RELATIONSHIP_WITH_TRANSFORMATION(#48)
SHAPE_REPRESENTATION_RELATIONSHIP()
);
#174=(
REPRESENTATION_RELATIONSHIP($,$,#27369,#27352)
REPRESENTATION_RELATIONSHIP_WITH_TRANSFORMATION(#49)
SHAPE_REPRESENTATION_RELATIONSHIP()
);
#175=(
REPRESENTATION_RELATIONSHIP($,$,#27370,#27352)
REPRESENTATION_RELATIONSHIP_WITH_TRANSFORMATION(#50)
SHAPE_REPRESENTATION_RELATIONSHIP()
);
#176=(
REPRESENTATION_RELATIONSHIP($,$,#27371,#27352)
REPRESENTATION_RELATIONSHIP_WITH_TRANSFORMATION(#51)
SHAPE_REPRESENTATION_RELATIONSHIP()
);
#177=(
REPRESENTATION_RELATIONSHIP($,$,#27372,#27352)
REPRESENTATION_RELATIONSHIP_WITH_TRANSFORMATION(#52)
SHAPE_REPRESENTATION_RELATIONSHIP()
);
#178=(
REPRESENTATION_RELATIONSHIP($,$,#27373,#27352)
REPRESENTATION_RELATIONSHIP_WITH_TRANSFORMATION(#53)
SHAPE_REPRESENTATION_RELATIONSHIP()
);
#179=(
REPRESENTATION_RELATIONSHIP($,$,#27374,#27352)
REPRESENTATION_RELATIONSHIP_WITH_TRANSFORMATION(#54)
SHAPE_REPRESENTATION_RELATIONSHIP()
);
#180=(
REPRESENTATION_RELATIONSHIP($,$,#27375,#27352)
REPRESENTATION_RELATIONSHIP_WITH_TRANSFORMATION(#55)
SHAPE_REPRESENTATION_RELATIONSHIP()
);
#181=(
REPRESENTATION_RELATIONSHIP($,$,#27376,#27352)
REPRESENTATION_RELATIONSHIP_WITH_TRANSFORMATION(#56)
SHAPE_REPRESENTATION_RELATIONSHIP()
);
#182=(
REPRESENTATION_RELATIONSHIP($,$,#27377,#27352)
REPRESENTATION_RELATIONSHIP_WITH_TRANSFORMATION(#57)
SHAPE_REPRESENTATION_RELATIONSHIP()
);
#183=(
REPRESENTATION_RELATIONSHIP($,$,#27378,#27352)
REPRESENTATION_RELATIONSHIP_WITH_TRANSFORMATION(#58)
SHAPE_REPRESENTATION_RELATIONSHIP()
);
#184=(
REPRESENTATION_RELATIONSHIP($,$,#27379,#27352)
REPRESENTATION_RELATIONSHIP_WITH_TRANSFORMATION(#59)
SHAPE_REPRESENTATION_RELATIONSHIP()
);
#185=(
REPRESENTATION_RELATIONSHIP($,$,#27425,#27352)
REPRESENTATION_RELATIONSHIP_WITH_TRANSFORMATION(#60)
SHAPE_REPRESENTATION_RELATIONSHIP()
);
#186=(
REPRESENTATION_RELATIONSHIP($,$,#27425,#27352)
REPRESENTATION_RELATIONSHIP_WITH_TRANSFORMATION(#61)
SHAPE_REPRESENTATION_RELATIONSHIP()
);
#187=(
REPRESENTATION_RELATIONSHIP($,$,#27425,#27352)
REPRESENTATION_RELATIONSHIP_WITH_TRANSFORMATION(#62)
SHAPE_REPRESENTATION_RELATIONSHIP()
);
#188=(
REPRESENTATION_RELATIONSHIP($,$,#27425,#27352)
REPRESENTATION_RELATIONSHIP_WITH_TRANSFORMATION(#63)
SHAPE_REPRESENTATION_RELATIONSHIP()
);
#189=(
REPRESENTATION_RELATIONSHIP($,$,#27380,#27352)
REPRESENTATION_RELATIONSHIP_WITH_TRANSFORMATION(#64)
SHAPE_REPRESENTATION_RELATIONSHIP()
);
#190=(
REPRESENTATION_RELATIONSHIP($,$,#27380,#27352)
REPRESENTATION_RELATIONSHIP_WITH_TRANSFORMATION(#65)
SHAPE_REPRESENTATION_RELATIONSHIP()
);
#191=(
REPRESENTATION_RELATIONSHIP($,$,#27399,#27352)
REPRESENTATION_RELATIONSHIP_WITH_TRANSFORMATION(#66)
SHAPE_REPRESENTATION_RELATIONSHIP()
);
#192=(
REPRESENTATION_RELATIONSHIP($,$,#27399,#27352)
REPRESENTATION_RELATIONSHIP_WITH_TRANSFORMATION(#67)
SHAPE_REPRESENTATION_RELATIONSHIP()
);
#193=(
REPRESENTATION_RELATIONSHIP($,$,#27399,#27352)
REPRESENTATION_RELATIONSHIP_WITH_TRANSFORMATION(#68)
SHAPE_REPRESENTATION_RELATIONSHIP()
);
#194=(
REPRESENTATION_RELATIONSHIP($,$,#27399,#27352)
REPRESENTATION_RELATIONSHIP_WITH_TRANSFORMATION(#69)
SHAPE_REPRESENTATION_RELATIONSHIP()
);
#195=(
REPRESENTATION_RELATIONSHIP($,$,#27399,#27352)
REPRESENTATION_RELATIONSHIP_WITH_TRANSFORMATION(#70)
SHAPE_REPRESENTATION_RELATIONSHIP()
);
#196=(
REPRESENTATION_RELATIONSHIP($,$,#27399,#27352)
REPRESENTATION_RELATIONSHIP_WITH_TRANSFORMATION(#71)
SHAPE_REPRESENTATION_RELATIONSHIP()
);
#197=(
REPRESENTATION_RELATIONSHIP($,$,#27399,#27352)
REPRESENTATION_RELATIONSHIP_WITH_TRANSFORMATION(#72)
SHAPE_REPRESENTATION_RELATIONSHIP()
);
#198=(
REPRESENTATION_RELATIONSHIP($,$,#27399,#27352)
REPRESENTATION_RELATIONSHIP_WITH_TRANSFORMATION(#73)
SHAPE_REPRESENTATION_RELATIONSHIP()
);
#199=(
REPRESENTATION_RELATIONSHIP($,$,#27386,#27352)
REPRESENTATION_RELATIONSHIP_WITH_TRANSFORMATION(#74)
SHAPE_REPRESENTATION_RELATIONSHIP()
);
#200=(
REPRESENTATION_RELATIONSHIP($,$,#27386,#27352)
REPRESENTATION_RELATIONSHIP_WITH_TRANSFORMATION(#75)
SHAPE_REPRESENTATION_RELATIONSHIP()
);
#201=(
REPRESENTATION_RELATIONSHIP($,$,#27386,#27352)
REPRESENTATION_RELATIONSHIP_WITH_TRANSFORMATION(#76)
SHAPE_REPRESENTATION_RELATIONSHIP()
);
#202=(
REPRESENTATION_RELATIONSHIP($,$,#27386,#27352)
REPRESENTATION_RELATIONSHIP_WITH_TRANSFORMATION(#77)
SHAPE_REPRESENTATION_RELATIONSHIP()
);
#203=(
REPRESENTATION_RELATIONSHIP($,$,#27387,#27352)
REPRESENTATION_RELATIONSHIP_WITH_TRANSFORMATION(#78)
SHAPE_REPRESENTATION_RELATIONSHIP()
);
#204=(
REPRESENTATION_RELATIONSHIP($,$,#27387,#27352)
REPRESENTATION_RELATIONSHIP_WITH_TRANSFORMATION(#79)
SHAPE_REPRESENTATION_RELATIONSHIP()
);
#205=(
REPRESENTATION_RELATIONSHIP($,$,#27399,#27352)
REPRESENTATION_RELATIONSHIP_WITH_TRANSFORMATION(#80)
SHAPE_REPRESENTATION_RELATIONSHIP()
);
#206=(
REPRESENTATION_RELATIONSHIP($,$,#27399,#27352)
REPRESENTATION_RELATIONSHIP_WITH_TRANSFORMATION(#81)
SHAPE_REPRESENTATION_RELATIONSHIP()
);
#207=(
REPRESENTATION_RELATIONSHIP($,$,#27399,#27352)
REPRESENTATION_RELATIONSHIP_WITH_TRANSFORMATION(#82)
SHAPE_REPRESENTATION_RELATIONSHIP()
);
#208=(
REPRESENTATION_RELATIONSHIP($,$,#27399,#27352)
REPRESENTATION_RELATIONSHIP_WITH_TRANSFORMATION(#83)
SHAPE_REPRESENTATION_RELATIONSHIP()
);
#209=(
REPRESENTATION_RELATIONSHIP($,$,#27399,#27352)
REPRESENTATION_RELATIONSHIP_WITH_TRANSFORMATION(#84)
SHAPE_REPRESENTATION_RELATIONSHIP()
);
#210=(
REPRESENTATION_RELATIONSHIP($,$,#27399,#27352)
REPRESENTATION_RELATIONSHIP_WITH_TRANSFORMATION(#85)
SHAPE_REPRESENTATION_RELATIONSHIP()
);
#211=(
REPRESENTATION_RELATIONSHIP($,$,#27399,#27352)
REPRESENTATION_RELATIONSHIP_WITH_TRANSFORMATION(#86)
SHAPE_REPRESENTATION_RELATIONSHIP()
);
#212=(
REPRESENTATION_RELATIONSHIP($,$,#27399,#27352)
REPRESENTATION_RELATIONSHIP_WITH_TRANSFORMATION(#87)
SHAPE_REPRESENTATION_RELATIONSHIP()
);
#213=(
REPRESENTATION_RELATIONSHIP($,$,#27393,#27352)
REPRESENTATION_RELATIONSHIP_WITH_TRANSFORMATION(#88)
SHAPE_REPRESENTATION_RELATIONSHIP()
);
#214=(
REPRESENTATION_RELATIONSHIP($,$,#27393,#27352)
REPRESENTATION_RELATIONSHIP_WITH_TRANSFORMATION(#89)
SHAPE_REPRESENTATION_RELATIONSHIP()
);
#215=(
REPRESENTATION_RELATIONSHIP($,$,#27393,#27352)
REPRESENTATION_RELATIONSHIP_WITH_TRANSFORMATION(#90)
SHAPE_REPRESENTATION_RELATIONSHIP()
);
#216=(
REPRESENTATION_RELATIONSHIP($,$,#27393,#27352)
REPRESENTATION_RELATIONSHIP_WITH_TRANSFORMATION(#91)
SHAPE_REPRESENTATION_RELATIONSHIP()
);
#217=(
REPRESENTATION_RELATIONSHIP($,$,#27394,#27352)
REPRESENTATION_RELATIONSHIP_WITH_TRANSFORMATION(#92)
SHAPE_REPRESENTATION_RELATIONSHIP()
);
#218=(
REPRESENTATION_RELATIONSHIP($,$,#27397,#27352)
REPRESENTATION_RELATIONSHIP_WITH_TRANSFORMATION(#93)
SHAPE_REPRESENTATION_RELATIONSHIP()
);
#219=(
REPRESENTATION_RELATIONSHIP($,$,#27398,#27352)
REPRESENTATION_RELATIONSHIP_WITH_TRANSFORMATION(#94)
SHAPE_REPRESENTATION_RELATIONSHIP()
);
#220=(
REPRESENTATION_RELATIONSHIP($,$,#27397,#27352)
REPRESENTATION_RELATIONSHIP_WITH_TRANSFORMATION(#95)
SHAPE_REPRESENTATION_RELATIONSHIP()
);
#221=(
REPRESENTATION_RELATIONSHIP($,$,#27398,#27352)
REPRESENTATION_RELATIONSHIP_WITH_TRANSFORMATION(#96)
SHAPE_REPRESENTATION_RELATIONSHIP()
);
#222=(
REPRESENTATION_RELATIONSHIP($,$,#27393,#27352)
REPRESENTATION_RELATIONSHIP_WITH_TRANSFORMATION(#97)
SHAPE_REPRESENTATION_RELATIONSHIP()
);
#223=(
REPRESENTATION_RELATIONSHIP($,$,#27393,#27352)
REPRESENTATION_RELATIONSHIP_WITH_TRANSFORMATION(#98)
SHAPE_REPRESENTATION_RELATIONSHIP()
);
#224=(
REPRESENTATION_RELATIONSHIP($,$,#27393,#27352)
REPRESENTATION_RELATIONSHIP_WITH_TRANSFORMATION(#99)
SHAPE_REPRESENTATION_RELATIONSHIP()
);
#225=(
REPRESENTATION_RELATIONSHIP($,$,#27393,#27352)
REPRESENTATION_RELATIONSHIP_WITH_TRANSFORMATION(#100)
SHAPE_REPRESENTATION_RELATIONSHIP()
);
#226=(
REPRESENTATION_RELATIONSHIP($,$,#27394,#27352)
REPRESENTATION_RELATIONSHIP_WITH_TRANSFORMATION(#101)
SHAPE_REPRESENTATION_RELATIONSHIP()
);
#227=(
REPRESENTATION_RELATIONSHIP($,$,#27397,#27352)
REPRESENTATION_RELATIONSHIP_WITH_TRANSFORMATION(#102)
SHAPE_REPRESENTATION_RELATIONSHIP()
);
#228=(
REPRESENTATION_RELATIONSHIP($,$,#27398,#27352)
REPRESENTATION_RELATIONSHIP_WITH_TRANSFORMATION(#103)
SHAPE_REPRESENTATION_RELATIONSHIP()
);
#229=(
REPRESENTATION_RELATIONSHIP($,$,#27397,#27352)
REPRESENTATION_RELATIONSHIP_WITH_TRANSFORMATION(#104)
SHAPE_REPRESENTATION_RELATIONSHIP()
);
#230=(
REPRESENTATION_RELATIONSHIP($,$,#27398,#27352)
REPRESENTATION_RELATIONSHIP_WITH_TRANSFORMATION(#105)
SHAPE_REPRESENTATION_RELATIONSHIP()
);
#231=(
REPRESENTATION_RELATIONSHIP($,$,#27425,#27352)
REPRESENTATION_RELATIONSHIP_WITH_TRANSFORMATION(#106)
SHAPE_REPRESENTATION_RELATIONSHIP()
);
#232=(
REPRESENTATION_RELATIONSHIP($,$,#27425,#27352)
REPRESENTATION_RELATIONSHIP_WITH_TRANSFORMATION(#107)
SHAPE_REPRESENTATION_RELATIONSHIP()
);
#233=(
REPRESENTATION_RELATIONSHIP($,$,#27399,#27352)
REPRESENTATION_RELATIONSHIP_WITH_TRANSFORMATION(#108)
SHAPE_REPRESENTATION_RELATIONSHIP()
);
#234=(
REPRESENTATION_RELATIONSHIP($,$,#27399,#27352)
REPRESENTATION_RELATIONSHIP_WITH_TRANSFORMATION(#109)
SHAPE_REPRESENTATION_RELATIONSHIP()
);
#235=(
REPRESENTATION_RELATIONSHIP($,$,#27399,#27352)
REPRESENTATION_RELATIONSHIP_WITH_TRANSFORMATION(#110)
SHAPE_REPRESENTATION_RELATIONSHIP()
);
#236=(
REPRESENTATION_RELATIONSHIP($,$,#27399,#27352)
REPRESENTATION_RELATIONSHIP_WITH_TRANSFORMATION(#111)
SHAPE_REPRESENTATION_RELATIONSHIP()
);
#237=(
REPRESENTATION_RELATIONSHIP($,$,#27401,#27400)
REPRESENTATION_RELATIONSHIP_WITH_TRANSFORMATION(#112)
SHAPE_REPRESENTATION_RELATIONSHIP()
);
#238=(
REPRESENTATION_RELATIONSHIP($,$,#27402,#27400)
REPRESENTATION_RELATIONSHIP_WITH_TRANSFORMATION(#113)
SHAPE_REPRESENTATION_RELATIONSHIP()
);
#239=(
REPRESENTATION_RELATIONSHIP($,$,#27403,#27400)
REPRESENTATION_RELATIONSHIP_WITH_TRANSFORMATION(#114)
SHAPE_REPRESENTATION_RELATIONSHIP()
);
#240=(
REPRESENTATION_RELATIONSHIP($,$,#27404,#27400)
REPRESENTATION_RELATIONSHIP_WITH_TRANSFORMATION(#115)
SHAPE_REPRESENTATION_RELATIONSHIP()
);
#241=(
REPRESENTATION_RELATIONSHIP($,$,#27405,#27400)
REPRESENTATION_RELATIONSHIP_WITH_TRANSFORMATION(#116)
SHAPE_REPRESENTATION_RELATIONSHIP()
);
#242=(
REPRESENTATION_RELATIONSHIP($,$,#27406,#27400)
REPRESENTATION_RELATIONSHIP_WITH_TRANSFORMATION(#117)
SHAPE_REPRESENTATION_RELATIONSHIP()
);
#243=(
REPRESENTATION_RELATIONSHIP($,$,#27407,#27400)
REPRESENTATION_RELATIONSHIP_WITH_TRANSFORMATION(#118)
SHAPE_REPRESENTATION_RELATIONSHIP()
);
#244=(
REPRESENTATION_RELATIONSHIP($,$,#27408,#27400)
REPRESENTATION_RELATIONSHIP_WITH_TRANSFORMATION(#119)
SHAPE_REPRESENTATION_RELATIONSHIP()
);
#245=(
REPRESENTATION_RELATIONSHIP($,$,#27409,#27400)
REPRESENTATION_RELATIONSHIP_WITH_TRANSFORMATION(#120)
SHAPE_REPRESENTATION_RELATIONSHIP()
);
#246=(
REPRESENTATION_RELATIONSHIP($,$,#27425,#27400)
REPRESENTATION_RELATIONSHIP_WITH_TRANSFORMATION(#121)
SHAPE_REPRESENTATION_RELATIONSHIP()
);
#247=(
REPRESENTATION_RELATIONSHIP($,$,#27426,#27400)
REPRESENTATION_RELATIONSHIP_WITH_TRANSFORMATION(#122)
SHAPE_REPRESENTATION_RELATIONSHIP()
);
#248=(
REPRESENTATION_RELATIONSHIP($,$,#27426,#27400)
REPRESENTATION_RELATIONSHIP_WITH_TRANSFORMATION(#123)
SHAPE_REPRESENTATION_RELATIONSHIP()
);
#249=(
REPRESENTATION_RELATIONSHIP($,$,#27411,#27410)
REPRESENTATION_RELATIONSHIP_WITH_TRANSFORMATION(#124)
SHAPE_REPRESENTATION_RELATIONSHIP()
);
#250=(
REPRESENTATION_RELATIONSHIP($,$,#27412,#27410)
REPRESENTATION_RELATIONSHIP_WITH_TRANSFORMATION(#125)
SHAPE_REPRESENTATION_RELATIONSHIP()
);
#251=(
REPRESENTATION_RELATIONSHIP($,$,#27413,#27410)
REPRESENTATION_RELATIONSHIP_WITH_TRANSFORMATION(#126)
SHAPE_REPRESENTATION_RELATIONSHIP()
);
#252=(
REPRESENTATION_RELATIONSHIP($,$,#27414,#27410)
REPRESENTATION_RELATIONSHIP_WITH_TRANSFORMATION(#127)
SHAPE_REPRESENTATION_RELATIONSHIP()
);
#253=(
REPRESENTATION_RELATIONSHIP($,$,#27415,#27410)
REPRESENTATION_RELATIONSHIP_WITH_TRANSFORMATION(#128)
SHAPE_REPRESENTATION_RELATIONSHIP()
);
#254=(
REPRESENTATION_RELATIONSHIP($,$,#27416,#27410)
REPRESENTATION_RELATIONSHIP_WITH_TRANSFORMATION(#129)
SHAPE_REPRESENTATION_RELATIONSHIP()
);
#255=(
REPRESENTATION_RELATIONSHIP($,$,#27417,#27410)
REPRESENTATION_RELATIONSHIP_WITH_TRANSFORMATION(#130)
SHAPE_REPRESENTATION_RELATIONSHIP()
);
#256=(
REPRESENTATION_RELATIONSHIP($,$,#27418,#27410)
REPRESENTATION_RELATIONSHIP_WITH_TRANSFORMATION(#131)
SHAPE_REPRESENTATION_RELATIONSHIP()
);
#257=(
REPRESENTATION_RELATIONSHIP($,$,#27419,#27410)
REPRESENTATION_RELATIONSHIP_WITH_TRANSFORMATION(#132)
SHAPE_REPRESENTATION_RELATIONSHIP()
);
#258=(
REPRESENTATION_RELATIONSHIP($,$,#27420,#27410)
REPRESENTATION_RELATIONSHIP_WITH_TRANSFORMATION(#133)
SHAPE_REPRESENTATION_RELATIONSHIP()
);
#259=(
REPRESENTATION_RELATIONSHIP($,$,#27421,#27410)
REPRESENTATION_RELATIONSHIP_WITH_TRANSFORMATION(#134)
SHAPE_REPRESENTATION_RELATIONSHIP()
);
#260=(
REPRESENTATION_RELATIONSHIP($,$,#27422,#27410)
REPRESENTATION_RELATIONSHIP_WITH_TRANSFORMATION(#135)
SHAPE_REPRESENTATION_RELATIONSHIP()
);
#261=(
REPRESENTATION_RELATIONSHIP($,$,#27423,#27410)
REPRESENTATION_RELATIONSHIP_WITH_TRANSFORMATION(#136)
SHAPE_REPRESENTATION_RELATIONSHIP()
);
#262=(
REPRESENTATION_RELATIONSHIP($,$,#27424,#27410)
REPRESENTATION_RELATIONSHIP_WITH_TRANSFORMATION(#137)
SHAPE_REPRESENTATION_RELATIONSHIP()
);
#263=(
REPRESENTATION_RELATIONSHIP($,$,#27425,#27410)
REPRESENTATION_RELATIONSHIP_WITH_TRANSFORMATION(#138)
SHAPE_REPRESENTATION_RELATIONSHIP()
);
#264=(
REPRESENTATION_RELATIONSHIP($,$,#27426,#27410)
REPRESENTATION_RELATIONSHIP_WITH_TRANSFORMATION(#139)
SHAPE_REPRESENTATION_RELATIONSHIP()
);
#265=(
REPRESENTATION_RELATIONSHIP($,$,#27426,#27410)
REPRESENTATION_RELATIONSHIP_WITH_TRANSFORMATION(#140)
SHAPE_REPRESENTATION_RELATIONSHIP()
);
#266=(
REPRESENTATION_RELATIONSHIP($,$,#27426,#27410)
REPRESENTATION_RELATIONSHIP_WITH_TRANSFORMATION(#141)
SHAPE_REPRESENTATION_RELATIONSHIP()
);
#267=(
REPRESENTATION_RELATIONSHIP($,$,#27426,#27410)
REPRESENTATION_RELATIONSHIP_WITH_TRANSFORMATION(#142)
SHAPE_REPRESENTATION_RELATIONSHIP()
);
#268=(
REPRESENTATION_RELATIONSHIP($,$,#27352,#27351)
REPRESENTATION_RELATIONSHIP_WITH_TRANSFORMATION(#143)
SHAPE_REPRESENTATION_RELATIONSHIP()
);
#269=(
REPRESENTATION_RELATIONSHIP($,$,#27400,#27351)
REPRESENTATION_RELATIONSHIP_WITH_TRANSFORMATION(#144)
SHAPE_REPRESENTATION_RELATIONSHIP()
);
#270=(
REPRESENTATION_RELATIONSHIP($,$,#27410,#27351)
REPRESENTATION_RELATIONSHIP_WITH_TRANSFORMATION(#145)
SHAPE_REPRESENTATION_RELATIONSHIP()
);
#271=CONTEXT_DEPENDENT_SHAPE_REPRESENTATION(#146,#27185);
#272=CONTEXT_DEPENDENT_SHAPE_REPRESENTATION(#147,#27186);
#273=CONTEXT_DEPENDENT_SHAPE_REPRESENTATION(#148,#27187);
#274=CONTEXT_DEPENDENT_SHAPE_REPRESENTATION(#149,#27188);
#275=CONTEXT_DEPENDENT_SHAPE_REPRESENTATION(#150,#27189);
#276=CONTEXT_DEPENDENT_SHAPE_REPRESENTATION(#151,#27197);
#277=CONTEXT_DEPENDENT_SHAPE_REPRESENTATION(#152,#27198);
#278=CONTEXT_DEPENDENT_SHAPE_REPRESENTATION(#153,#27199);
#279=CONTEXT_DEPENDENT_SHAPE_REPRESENTATION(#154,#27200);
#280=CONTEXT_DEPENDENT_SHAPE_REPRESENTATION(#155,#27201);
#281=CONTEXT_DEPENDENT_SHAPE_REPRESENTATION(#156,#27206);
#282=CONTEXT_DEPENDENT_SHAPE_REPRESENTATION(#157,#27207);
#283=CONTEXT_DEPENDENT_SHAPE_REPRESENTATION(#158,#27237);
#284=CONTEXT_DEPENDENT_SHAPE_REPRESENTATION(#159,#27238);
#285=CONTEXT_DEPENDENT_SHAPE_REPRESENTATION(#160,#27239);
#286=CONTEXT_DEPENDENT_SHAPE_REPRESENTATION(#161,#27240);
#287=CONTEXT_DEPENDENT_SHAPE_REPRESENTATION(#162,#27241);
#288=CONTEXT_DEPENDENT_SHAPE_REPRESENTATION(#163,#27242);
#289=CONTEXT_DEPENDENT_SHAPE_REPRESENTATION(#164,#27243);
#290=CONTEXT_DEPENDENT_SHAPE_REPRESENTATION(#165,#27244);
#291=CONTEXT_DEPENDENT_SHAPE_REPRESENTATION(#166,#27245);
#292=CONTEXT_DEPENDENT_SHAPE_REPRESENTATION(#167,#27246);
#293=CONTEXT_DEPENDENT_SHAPE_REPRESENTATION(#168,#27247);
#294=CONTEXT_DEPENDENT_SHAPE_REPRESENTATION(#169,#27248);
#295=CONTEXT_DEPENDENT_SHAPE_REPRESENTATION(#170,#27249);
#296=CONTEXT_DEPENDENT_SHAPE_REPRESENTATION(#171,#27250);
#297=CONTEXT_DEPENDENT_SHAPE_REPRESENTATION(#172,#27251);
#298=CONTEXT_DEPENDENT_SHAPE_REPRESENTATION(#173,#27252);
#299=CONTEXT_DEPENDENT_SHAPE_REPRESENTATION(#174,#27253);
#300=CONTEXT_DEPENDENT_SHAPE_REPRESENTATION(#175,#27254);
#301=CONTEXT_DEPENDENT_SHAPE_REPRESENTATION(#176,#27255);
#302=CONTEXT_DEPENDENT_SHAPE_REPRESENTATION(#177,#27256);
#303=CONTEXT_DEPENDENT_SHAPE_REPRESENTATION(#178,#27257);
#304=CONTEXT_DEPENDENT_SHAPE_REPRESENTATION(#179,#27258);
#305=CONTEXT_DEPENDENT_SHAPE_REPRESENTATION(#180,#27259);
#306=CONTEXT_DEPENDENT_SHAPE_REPRESENTATION(#181,#27260);
#307=CONTEXT_DEPENDENT_SHAPE_REPRESENTATION(#182,#27261);
#308=CONTEXT_DEPENDENT_SHAPE_REPRESENTATION(#183,#27262);
#309=CONTEXT_DEPENDENT_SHAPE_REPRESENTATION(#184,#27263);
#310=CONTEXT_DEPENDENT_SHAPE_REPRESENTATION(#185,#27264);
#311=CONTEXT_DEPENDENT_SHAPE_REPRESENTATION(#186,#27265);
#312=CONTEXT_DEPENDENT_SHAPE_REPRESENTATION(#187,#27266);
#313=CONTEXT_DEPENDENT_SHAPE_REPRESENTATION(#188,#27267);
#314=CONTEXT_DEPENDENT_SHAPE_REPRESENTATION(#189,#27268);
#315=CONTEXT_DEPENDENT_SHAPE_REPRESENTATION(#190,#27269);
#316=CONTEXT_DEPENDENT_SHAPE_REPRESENTATION(#191,#27270);
#317=CONTEXT_DEPENDENT_SHAPE_REPRESENTATION(#192,#27271);
#318=CONTEXT_DEPENDENT_SHAPE_REPRESENTATION(#193,#27272);
#319=CONTEXT_DEPENDENT_SHAPE_REPRESENTATION(#194,#27273);
#320=CONTEXT_DEPENDENT_SHAPE_REPRESENTATION(#195,#27274);
#321=CONTEXT_DEPENDENT_SHAPE_REPRESENTATION(#196,#27275);
#322=CONTEXT_DEPENDENT_SHAPE_REPRESENTATION(#197,#27276);
#323=CONTEXT_DEPENDENT_SHAPE_REPRESENTATION(#198,#27277);
#324=CONTEXT_DEPENDENT_SHAPE_REPRESENTATION(#199,#27278);
#325=CONTEXT_DEPENDENT_SHAPE_REPRESENTATION(#200,#27279);
#326=CONTEXT_DEPENDENT_SHAPE_REPRESENTATION(#201,#27280);
#327=CONTEXT_DEPENDENT_SHAPE_REPRESENTATION(#202,#27281);
#328=CONTEXT_DEPENDENT_SHAPE_REPRESENTATION(#203,#27282);
#329=CONTEXT_DEPENDENT_SHAPE_REPRESENTATION(#204,#27283);
#330=CONTEXT_DEPENDENT_SHAPE_REPRESENTATION(#205,#27284);
#331=CONTEXT_DEPENDENT_SHAPE_REPRESENTATION(#206,#27285);
#332=CONTEXT_DEPENDENT_SHAPE_REPRESENTATION(#207,#27286);
#333=CONTEXT_DEPENDENT_SHAPE_REPRESENTATION(#208,#27287);
#334=CONTEXT_DEPENDENT_SHAPE_REPRESENTATION(#209,#27288);
#335=CONTEXT_DEPENDENT_SHAPE_REPRESENTATION(#210,#27289);
#336=CONTEXT_DEPENDENT_SHAPE_REPRESENTATION(#211,#27290);
#337=CONTEXT_DEPENDENT_SHAPE_REPRESENTATION(#212,#27291);
#338=CONTEXT_DEPENDENT_SHAPE_REPRESENTATION(#213,#27292);
#339=CONTEXT_DEPENDENT_SHAPE_REPRESENTATION(#214,#27293);
#340=CONTEXT_DEPENDENT_SHAPE_REPRESENTATION(#215,#27294);
#341=CONTEXT_DEPENDENT_SHAPE_REPRESENTATION(#216,#27295);
#342=CONTEXT_DEPENDENT_SHAPE_REPRESENTATION(#217,#27296);
#343=CONTEXT_DEPENDENT_SHAPE_REPRESENTATION(#218,#27297);
#344=CONTEXT_DEPENDENT_SHAPE_REPRESENTATION(#219,#27298);
#345=CONTEXT_DEPENDENT_SHAPE_REPRESENTATION(#220,#27299);
#346=CONTEXT_DEPENDENT_SHAPE_REPRESENTATION(#221,#27300);
#347=CONTEXT_DEPENDENT_SHAPE_REPRESENTATION(#222,#27301);
#348=CONTEXT_DEPENDENT_SHAPE_REPRESENTATION(#223,#27302);
#349=CONTEXT_DEPENDENT_SHAPE_REPRESENTATION(#224,#27303);
#350=CONTEXT_DEPENDENT_SHAPE_REPRESENTATION(#225,#27304);
#351=CONTEXT_DEPENDENT_SHAPE_REPRESENTATION(#226,#27305);
#352=CONTEXT_DEPENDENT_SHAPE_REPRESENTATION(#227,#27306);
#353=CONTEXT_DEPENDENT_SHAPE_REPRESENTATION(#228,#27307);
#354=CONTEXT_DEPENDENT_SHAPE_REPRESENTATION(#229,#27308);
#355=CONTEXT_DEPENDENT_SHAPE_REPRESENTATION(#230,#27309);
#356=CONTEXT_DEPENDENT_SHAPE_REPRESENTATION(#231,#27310);
#357=CONTEXT_DEPENDENT_SHAPE_REPRESENTATION(#232,#27311);
#358=CONTEXT_DEPENDENT_SHAPE_REPRESENTATION(#233,#27312);
#359=CONTEXT_DEPENDENT_SHAPE_REPRESENTATION(#234,#27313);
#360=CONTEXT_DEPENDENT_SHAPE_REPRESENTATION(#235,#27314);
#361=CONTEXT_DEPENDENT_SHAPE_REPRESENTATION(#236,#27315);
#362=CONTEXT_DEPENDENT_SHAPE_REPRESENTATION(#237,#27317);
#363=CONTEXT_DEPENDENT_SHAPE_REPRESENTATION(#238,#27318);
#364=CONTEXT_DEPENDENT_SHAPE_REPRESENTATION(#239,#27319);
#365=CONTEXT_DEPENDENT_SHAPE_REPRESENTATION(#240,#27320);
#366=CONTEXT_DEPENDENT_SHAPE_REPRESENTATION(#241,#27321);
#367=CONTEXT_DEPENDENT_SHAPE_REPRESENTATION(#242,#27322);
#368=CONTEXT_DEPENDENT_SHAPE_REPRESENTATION(#243,#27323);
#369=CONTEXT_DEPENDENT_SHAPE_REPRESENTATION(#244,#27324);
#370=CONTEXT_DEPENDENT_SHAPE_REPRESENTATION(#245,#27325);
#371=CONTEXT_DEPENDENT_SHAPE_REPRESENTATION(#246,#27326);
#372=CONTEXT_DEPENDENT_SHAPE_REPRESENTATION(#247,#27327);
#373=CONTEXT_DEPENDENT_SHAPE_REPRESENTATION(#248,#27328);
#374=CONTEXT_DEPENDENT_SHAPE_REPRESENTATION(#249,#27329);
#375=CONTEXT_DEPENDENT_SHAPE_REPRESENTATION(#250,#27330);
#376=CONTEXT_DEPENDENT_SHAPE_REPRESENTATION(#251,#27331);
#377=CONTEXT_DEPENDENT_SHAPE_REPRESENTATION(#252,#27332);
#378=CONTEXT_DEPENDENT_SHAPE_REPRESENTATION(#253,#27333);
#379=CONTEXT_DEPENDENT_SHAPE_REPRESENTATION(#254,#27334);
#380=CONTEXT_DEPENDENT_SHAPE_REPRESENTATION(#255,#27335);
#381=CONTEXT_DEPENDENT_SHAPE_REPRESENTATION(#256,#27336);
#382=CONTEXT_DEPENDENT_SHAPE_REPRESENTATION(#257,#27337);
#383=CONTEXT_DEPENDENT_SHAPE_REPRESENTATION(#258,#27338);
#384=CONTEXT_DEPENDENT_SHAPE_REPRESENTATION(#259,#27339);
#385=CONTEXT_DEPENDENT_SHAPE_REPRESENTATION(#260,#27340);
#386=CONTEXT_DEPENDENT_SHAPE_REPRESENTATION(#261,#27341);
#387=CONTEXT_DEPENDENT_SHAPE_REPRESENTATION(#262,#27342);
#388=CONTEXT_DEPENDENT_SHAPE_REPRESENTATION(#263,#27343);
#389=CONTEXT_DEPENDENT_SHAPE_REPRESENTATION(#264,#27344);
#390=CONTEXT_DEPENDENT_SHAPE_REPRESENTATION(#265,#27345);
#391=CONTEXT_DEPENDENT_SHAPE_REPRESENTATION(#266,#27346);
#392=CONTEXT_DEPENDENT_SHAPE_REPRESENTATION(#267,#27347);
#393=CONTEXT_DEPENDENT_SHAPE_REPRESENTATION(#268,#27348);
#394=CONTEXT_DEPENDENT_SHAPE_REPRESENTATION(#269,#27349);
#395=CONTEXT_DEPENDENT_SHAPE_REPRESENTATION(#270,#27350);
#396=NEXT_ASSEMBLY_USAGE_OCCURRENCE('Inner ring:1','Inner ring:1',
'Inner ring:1',#27457,#27458,'Inner ring:1');
#397=NEXT_ASSEMBLY_USAGE_OCCURRENCE('Outer ring:1','Outer ring:1',
'Outer ring:1',#27457,#27459,'Outer ring:1');
#398=NEXT_ASSEMBLY_USAGE_OCCURRENCE('Balls:1','Balls:1','Balls:1',#27457,
#27460,'Balls:1');
#399=NEXT_ASSEMBLY_USAGE_OCCURRENCE('Cage:1','Cage:1','Cage:1',#27457,#27461,
'Cage:1');
#400=NEXT_ASSEMBLY_USAGE_OCCURRENCE('Seals 2RS:1','Seals 2RS:1',
'Seals 2RS:1',#27457,#27462,'Seals 2RS:1');
#401=NEXT_ASSEMBLY_USAGE_OCCURRENCE('Inner ring (1):1',
'Inner ring (1):1','Inner ring (1):1',#27464,#27465,'Inner ring (1):1');
#402=NEXT_ASSEMBLY_USAGE_OCCURRENCE('Outer ring (1):1',
'Outer ring (1):1','Outer ring (1):1',#27464,#27466,'Outer ring (1):1');
#403=NEXT_ASSEMBLY_USAGE_OCCURRENCE('Balls (1):1','Balls (1):1',
'Balls (1):1',#27464,#27467,'Balls (1):1');
#404=NEXT_ASSEMBLY_USAGE_OCCURRENCE('Cage (1):1','Cage (1):1',
'Cage (1):1',#27464,#27468,'Cage (1):1');
#405=NEXT_ASSEMBLY_USAGE_OCCURRENCE('Seals 2RS (1):1','Seals 2RS (1):1',
'Seals 2RS (1):1',#27464,#27469,'Seals 2RS (1):1');
#406=NEXT_ASSEMBLY_USAGE_OCCURRENCE('Housing:1','Housing:1','Housing:1',
#27471,#27472,'Housing:1');
#407=NEXT_ASSEMBLY_USAGE_OCCURRENCE('Insert bearing:1',
'Insert bearing:1','Insert bearing:1',#27471,#27473,'Insert bearing:1');
#408=NEXT_ASSEMBLY_USAGE_OCCURRENCE('Base:1','Base:1','Base:1',#27429,#27430,
'Base:1');
#409=NEXT_ASSEMBLY_USAGE_OCCURRENCE('Foot:1','Foot:1','Foot:1',#27429,#27431,
'Foot:1');
#410=NEXT_ASSEMBLY_USAGE_OCCURRENCE('Foot (1):1','Foot (1):1',
'Foot (1):1',#27429,#27432,'Foot (1):1');
#411=NEXT_ASSEMBLY_USAGE_OCCURRENCE('Fixed bearing block:1',
'Fixed bearing block:1','Fixed bearing block:1',#27429,#27433,
'Fixed bearing block:1');
#412=NEXT_ASSEMBLY_USAGE_OCCURRENCE('Input outer spacer:1',
'Input outer spacer:1','Input outer spacer:1',#27429,#27434,
'Input outer spacer:1');
#413=NEXT_ASSEMBLY_USAGE_OCCURRENCE('Input bearing cap:1',
'Input bearing cap:1','Input bearing cap:1',#27429,#27435,
'Input bearing cap:1');
#414=NEXT_ASSEMBLY_USAGE_OCCURRENCE('Input bearing cap (1):1',
'Input bearing cap (1):1','Input bearing cap (1):1',#27429,#27436,
'Input bearing cap (1):1');
#415=NEXT_ASSEMBLY_USAGE_OCCURRENCE('Sliding bearing block:1',
'Sliding bearing block:1','Sliding bearing block:1',#27429,#27437,
'Sliding bearing block:1');
#416=NEXT_ASSEMBLY_USAGE_OCCURRENCE('M4 clamp nut:1','M4 clamp nut:1',
'M4 clamp nut:1',#27429,#27438,'M4 clamp nut:1');
#417=NEXT_ASSEMBLY_USAGE_OCCURRENCE('M4 clamp nut (1):1',
'M4 clamp nut (1):1','M4 clamp nut (1):1',#27429,#27439,
'M4 clamp nut (1):1');
#418=NEXT_ASSEMBLY_USAGE_OCCURRENCE('M4 clamp nut (2):1',
'M4 clamp nut (2):1','M4 clamp nut (2):1',#27429,#27440,
'M4 clamp nut (2):1');
#419=NEXT_ASSEMBLY_USAGE_OCCURRENCE('M4 clamp nut (3):1',
'M4 clamp nut (3):1','M4 clamp nut (3):1',#27429,#27441,
'M4 clamp nut (3):1');
#420=NEXT_ASSEMBLY_USAGE_OCCURRENCE('Output outer spacer:1',
'Output outer spacer:1','Output outer spacer:1',#27429,#27442,
'Output outer spacer:1');
#421=NEXT_ASSEMBLY_USAGE_OCCURRENCE('Output bearing cap:1',
'Output bearing cap:1','Output bearing cap:1',#27429,#27443,
'Output bearing cap:1');
#422=NEXT_ASSEMBLY_USAGE_OCCURRENCE('Output bearing cap (1):1',
'Output bearing cap (1):1','Output bearing cap (1):1',#27429,#27444,
'Output bearing cap (1):1');
#423=NEXT_ASSEMBLY_USAGE_OCCURRENCE('Timing belt backing envelope:1',
'Timing belt backing envelope:1','Timing belt backing envelope:1',#27429,
#27445,'Timing belt backing envelope:1');
#424=NEXT_ASSEMBLY_USAGE_OCCURRENCE('Drum bearing riser:1',
'Drum bearing riser:1','Drum bearing riser:1',#27429,#27446,
'Drum bearing riser:1');
#425=NEXT_ASSEMBLY_USAGE_OCCURRENCE('Bearing mounting bush:1',
'Bearing mounting bush:1','Bearing mounting bush:1',#27429,#27447,
'Bearing mounting bush:1');
#426=NEXT_ASSEMBLY_USAGE_OCCURRENCE('Bearing mounting bush (1):1',
'Bearing mounting bush (1):1','Bearing mounting bush (1):1',#27429,#27448,
'Bearing mounting bush (1):1');
#427=NEXT_ASSEMBLY_USAGE_OCCURRENCE('Drum bearing riser (1):1',
'Drum bearing riser (1):1','Drum bearing riser (1):1',#27429,#27449,
'Drum bearing riser (1):1');
#428=NEXT_ASSEMBLY_USAGE_OCCURRENCE('Bearing mounting bush (2):1',
'Bearing mounting bush (2):1','Bearing mounting bush (2):1',#27429,#27450,
'Bearing mounting bush (2):1');
#429=NEXT_ASSEMBLY_USAGE_OCCURRENCE('Bearing mounting bush (3):1',
'Bearing mounting bush (3):1','Bearing mounting bush (3):1',#27429,#27451,
'Bearing mounting bush (3):1');
#430=NEXT_ASSEMBLY_USAGE_OCCURRENCE('Motor pedestal:1',
'Motor pedestal:1','Motor pedestal:1',#27429,#27452,'Motor pedestal:1');
#431=NEXT_ASSEMBLY_USAGE_OCCURRENCE('Motor envelope:1',
'Motor envelope:1','Motor envelope:1',#27429,#27453,'Motor envelope:1');
#432=NEXT_ASSEMBLY_USAGE_OCCURRENCE('Guard post:1','Guard post:1',
'Guard post:1',#27429,#27454,'Guard post:1');
#433=NEXT_ASSEMBLY_USAGE_OCCURRENCE('Guard post (1):1',
'Guard post (1):1','Guard post (1):1',#27429,#27455,'Guard post (1):1');
#434=NEXT_ASSEMBLY_USAGE_OCCURRENCE('Belt guard:1','Belt guard:1',
'Belt guard:1',#27429,#27456,'Belt guard:1');
#435=NEXT_ASSEMBLY_USAGE_OCCURRENCE('Cap Screw - M4x16:2',
'Cap Screw - M4x16:2','Cap Screw - M4x16:2',#27429,#27502,
'Cap Screw - M4x16:2');
#436=NEXT_ASSEMBLY_USAGE_OCCURRENCE('Cap Screw - M4x16:3',
'Cap Screw - M4x16:3','Cap Screw - M4x16:3',#27429,#27502,
'Cap Screw - M4x16:3');
#437=NEXT_ASSEMBLY_USAGE_OCCURRENCE('Cap Screw - M4x16:4',
'Cap Screw - M4x16:4','Cap Screw - M4x16:4',#27429,#27502,
'Cap Screw - M4x16:4');
#438=NEXT_ASSEMBLY_USAGE_OCCURRENCE('Cap Screw - M4x16:5',
'Cap Screw - M4x16:5','Cap Screw - M4x16:5',#27429,#27502,
'Cap Screw - M4x16:5');
#439=NEXT_ASSEMBLY_USAGE_OCCURRENCE(
'Sealed Ball Bearing - 10 x 30 x 9 mm:2',
'Sealed Ball Bearing - 10 x 30 x 9 mm:2',
'Sealed Ball Bearing - 10 x 30 x 9 mm:2',#27429,#27457,
'Sealed Ball Bearing - 10 x 30 x 9 mm:2');
#440=NEXT_ASSEMBLY_USAGE_OCCURRENCE(
'Sealed Ball Bearing - 10 x 30 x 9 mm:3',
'Sealed Ball Bearing - 10 x 30 x 9 mm:3',
'Sealed Ball Bearing - 10 x 30 x 9 mm:3',#27429,#27457,
'Sealed Ball Bearing - 10 x 30 x 9 mm:3');
#441=NEXT_ASSEMBLY_USAGE_OCCURRENCE('M4x10 Cap Screw:2',
'M4x10 Cap Screw:2','M4x10 Cap Screw:2',#27429,#27476,
'M4x10 Cap Screw:2');
#442=NEXT_ASSEMBLY_USAGE_OCCURRENCE('M4x10 Cap Screw:3',
'M4x10 Cap Screw:3','M4x10 Cap Screw:3',#27429,#27476,
'M4x10 Cap Screw:3');
#443=NEXT_ASSEMBLY_USAGE_OCCURRENCE('M4x10 Cap Screw:4',
'M4x10 Cap Screw:4','M4x10 Cap Screw:4',#27429,#27476,
'M4x10 Cap Screw:4');
#444=NEXT_ASSEMBLY_USAGE_OCCURRENCE('M4x10 Cap Screw:5',
'M4x10 Cap Screw:5','M4x10 Cap Screw:5',#27429,#27476,
'M4x10 Cap Screw:5');
#445=NEXT_ASSEMBLY_USAGE_OCCURRENCE('M4x10 Cap Screw:6',
'M4x10 Cap Screw:6','M4x10 Cap Screw:6',#27429,#27476,
'M4x10 Cap Screw:6');
#446=NEXT_ASSEMBLY_USAGE_OCCURRENCE('M4x10 Cap Screw:7',
'M4x10 Cap Screw:7','M4x10 Cap Screw:7',#27429,#27476,
'M4x10 Cap Screw:7');
#447=NEXT_ASSEMBLY_USAGE_OCCURRENCE('M4x10 Cap Screw:8',
'M4x10 Cap Screw:8','M4x10 Cap Screw:8',#27429,#27476,
'M4x10 Cap Screw:8');
#448=NEXT_ASSEMBLY_USAGE_OCCURRENCE('M4x10 Cap Screw:9',
'M4x10 Cap Screw:9','M4x10 Cap Screw:9',#27429,#27476,
'M4x10 Cap Screw:9');
#449=NEXT_ASSEMBLY_USAGE_OCCURRENCE('M4x30 mounting screw:2',
'M4x30 mounting screw:2','M4x30 mounting screw:2',#27429,#27463,
'M4x30 mounting screw:2');
#450=NEXT_ASSEMBLY_USAGE_OCCURRENCE('M4x30 mounting screw:3',
'M4x30 mounting screw:3','M4x30 mounting screw:3',#27429,#27463,
'M4x30 mounting screw:3');
#451=NEXT_ASSEMBLY_USAGE_OCCURRENCE('M4x30 mounting screw:4',
'M4x30 mounting screw:4','M4x30 mounting screw:4',#27429,#27463,
'M4x30 mounting screw:4');
#452=NEXT_ASSEMBLY_USAGE_OCCURRENCE('M4x30 mounting screw:5',
'M4x30 mounting screw:5','M4x30 mounting screw:5',#27429,#27463,
'M4x30 mounting screw:5');
#453=NEXT_ASSEMBLY_USAGE_OCCURRENCE(
'Sealed Ball Bearing - 12 x 32 x 10 mm:2',
'Sealed Ball Bearing - 12 x 32 x 10 mm:2',
'Sealed Ball Bearing - 12 x 32 x 10 mm:2',#27429,#27464,
'Sealed Ball Bearing - 12 x 32 x 10 mm:2');
#454=NEXT_ASSEMBLY_USAGE_OCCURRENCE(
'Sealed Ball Bearing - 12 x 32 x 10 mm:3',
'Sealed Ball Bearing - 12 x 32 x 10 mm:3',
'Sealed Ball Bearing - 12 x 32 x 10 mm:3',#27429,#27464,
'Sealed Ball Bearing - 12 x 32 x 10 mm:3');
#455=NEXT_ASSEMBLY_USAGE_OCCURRENCE('M4x10 Cap Screw:10',
'M4x10 Cap Screw:10','M4x10 Cap Screw:10',#27429,#27476,
'M4x10 Cap Screw:10');
#456=NEXT_ASSEMBLY_USAGE_OCCURRENCE('M4x10 Cap Screw:11',
'M4x10 Cap Screw:11','M4x10 Cap Screw:11',#27429,#27476,
'M4x10 Cap Screw:11');
#457=NEXT_ASSEMBLY_USAGE_OCCURRENCE('M4x10 Cap Screw:12',
'M4x10 Cap Screw:12','M4x10 Cap Screw:12',#27429,#27476,
'M4x10 Cap Screw:12');
#458=NEXT_ASSEMBLY_USAGE_OCCURRENCE('M4x10 Cap Screw:13',
'M4x10 Cap Screw:13','M4x10 Cap Screw:13',#27429,#27476,
'M4x10 Cap Screw:13');
#459=NEXT_ASSEMBLY_USAGE_OCCURRENCE('M4x10 Cap Screw:14',
'M4x10 Cap Screw:14','M4x10 Cap Screw:14',#27429,#27476,
'M4x10 Cap Screw:14');
#460=NEXT_ASSEMBLY_USAGE_OCCURRENCE('M4x10 Cap Screw:15',
'M4x10 Cap Screw:15','M4x10 Cap Screw:15',#27429,#27476,
'M4x10 Cap Screw:15');
#461=NEXT_ASSEMBLY_USAGE_OCCURRENCE('M4x10 Cap Screw:16',
'M4x10 Cap Screw:16','M4x10 Cap Screw:16',#27429,#27476,
'M4x10 Cap Screw:16');
#462=NEXT_ASSEMBLY_USAGE_OCCURRENCE('M4x10 Cap Screw:17',
'M4x10 Cap Screw:17','M4x10 Cap Screw:17',#27429,#27476,
'M4x10 Cap Screw:17');
#463=NEXT_ASSEMBLY_USAGE_OCCURRENCE('Cap Screw - M5x20:2',
'Cap Screw - M5x20:2','Cap Screw - M5x20:2',#27429,#27470,
'Cap Screw - M5x20:2');
#464=NEXT_ASSEMBLY_USAGE_OCCURRENCE('Cap Screw - M5x20:3',
'Cap Screw - M5x20:3','Cap Screw - M5x20:3',#27429,#27470,
'Cap Screw - M5x20:3');
#465=NEXT_ASSEMBLY_USAGE_OCCURRENCE('Cap Screw - M5x20:4',
'Cap Screw - M5x20:4','Cap Screw - M5x20:4',#27429,#27470,
'Cap Screw - M5x20:4');
#466=NEXT_ASSEMBLY_USAGE_OCCURRENCE('Cap Screw - M5x20:5',
'Cap Screw - M5x20:5','Cap Screw - M5x20:5',#27429,#27470,
'Cap Screw - M5x20:5');
#467=NEXT_ASSEMBLY_USAGE_OCCURRENCE(
'Pillow Block Bearing - 20 mm Bore:2',
'Pillow Block Bearing - 20 mm Bore:2',
'Pillow Block Bearing - 20 mm Bore:2',#27429,#27471,
'Pillow Block Bearing - 20 mm Bore:2');
#468=NEXT_ASSEMBLY_USAGE_OCCURRENCE('Flat Washer - M8:2',
'Flat Washer - M8:2','Flat Washer - M8:2',#27429,#27474,
'Flat Washer - M8:2');
#469=NEXT_ASSEMBLY_USAGE_OCCURRENCE('M8x25 Bolt:2','M8x25 Bolt:2',
'M8x25 Bolt:2',#27429,#27475,'M8x25 Bolt:2');
#470=NEXT_ASSEMBLY_USAGE_OCCURRENCE('Flat Washer - M8:3',
'Flat Washer - M8:3','Flat Washer - M8:3',#27429,#27474,
'Flat Washer - M8:3');
#471=NEXT_ASSEMBLY_USAGE_OCCURRENCE('M8x25 Bolt:3','M8x25 Bolt:3',
'M8x25 Bolt:3',#27429,#27475,'M8x25 Bolt:3');
#472=NEXT_ASSEMBLY_USAGE_OCCURRENCE('Cap Screw - M5x20:6',
'Cap Screw - M5x20:6','Cap Screw - M5x20:6',#27429,#27470,
'Cap Screw - M5x20:6');
#473=NEXT_ASSEMBLY_USAGE_OCCURRENCE('Cap Screw - M5x20:7',
'Cap Screw - M5x20:7','Cap Screw - M5x20:7',#27429,#27470,
'Cap Screw - M5x20:7');
#474=NEXT_ASSEMBLY_USAGE_OCCURRENCE('Cap Screw - M5x20:8',
'Cap Screw - M5x20:8','Cap Screw - M5x20:8',#27429,#27470,
'Cap Screw - M5x20:8');
#475=NEXT_ASSEMBLY_USAGE_OCCURRENCE('Cap Screw - M5x20:9',
'Cap Screw - M5x20:9','Cap Screw - M5x20:9',#27429,#27470,
'Cap Screw - M5x20:9');
#476=NEXT_ASSEMBLY_USAGE_OCCURRENCE(
'Pillow Block Bearing - 20 mm Bore:3',
'Pillow Block Bearing - 20 mm Bore:3',
'Pillow Block Bearing - 20 mm Bore:3',#27429,#27471,
'Pillow Block Bearing - 20 mm Bore:3');
#477=NEXT_ASSEMBLY_USAGE_OCCURRENCE('Flat Washer - M8:4',
'Flat Washer - M8:4','Flat Washer - M8:4',#27429,#27474,
'Flat Washer - M8:4');
#478=NEXT_ASSEMBLY_USAGE_OCCURRENCE('M8x25 Bolt:4','M8x25 Bolt:4',
'M8x25 Bolt:4',#27429,#27475,'M8x25 Bolt:4');
#479=NEXT_ASSEMBLY_USAGE_OCCURRENCE('Flat Washer - M8:5',
'Flat Washer - M8:5','Flat Washer - M8:5',#27429,#27474,
'Flat Washer - M8:5');
#480=NEXT_ASSEMBLY_USAGE_OCCURRENCE('M8x25 Bolt:5','M8x25 Bolt:5',
'M8x25 Bolt:5',#27429,#27475,'M8x25 Bolt:5');
#481=NEXT_ASSEMBLY_USAGE_OCCURRENCE('Cap Screw - M4x16:8',
'Cap Screw - M4x16:8','Cap Screw - M4x16:8',#27429,#27502,
'Cap Screw - M4x16:8');
#482=NEXT_ASSEMBLY_USAGE_OCCURRENCE('Cap Screw - M4x16:9',
'Cap Screw - M4x16:9','Cap Screw - M4x16:9',#27429,#27502,
'Cap Screw - M4x16:9');
#483=NEXT_ASSEMBLY_USAGE_OCCURRENCE('M4x10 Cap Screw:18',
'M4x10 Cap Screw:18','M4x10 Cap Screw:18',#27429,#27476,
'M4x10 Cap Screw:18');
#484=NEXT_ASSEMBLY_USAGE_OCCURRENCE('M4x10 Cap Screw:19',
'M4x10 Cap Screw:19','M4x10 Cap Screw:19',#27429,#27476,
'M4x10 Cap Screw:19');
#485=NEXT_ASSEMBLY_USAGE_OCCURRENCE('M4x10 Cap Screw:20',
'M4x10 Cap Screw:20','M4x10 Cap Screw:20',#27429,#27476,
'M4x10 Cap Screw:20');
#486=NEXT_ASSEMBLY_USAGE_OCCURRENCE('M4x10 Cap Screw:21',
'M4x10 Cap Screw:21','M4x10 Cap Screw:21',#27429,#27476,
'M4x10 Cap Screw:21');
#487=NEXT_ASSEMBLY_USAGE_OCCURRENCE('Input shaft:1','Input shaft:1',
'Input shaft:1',#27477,#27478,'Input shaft:1');
#488=NEXT_ASSEMBLY_USAGE_OCCURRENCE('Input inner spacer:1',
'Input inner spacer:1','Input inner spacer:1',#27477,#27479,
'Input inner spacer:1');
#489=NEXT_ASSEMBLY_USAGE_OCCURRENCE('Input inner sleeve:1',
'Input inner sleeve:1','Input inner sleeve:1',#27477,#27480,
'Input inner sleeve:1');
#490=NEXT_ASSEMBLY_USAGE_OCCURRENCE('Input M3 set screw:1',
'Input M3 set screw:1','Input M3 set screw:1',#27477,#27481,
'Input M3 set screw:1');
#491=NEXT_ASSEMBLY_USAGE_OCCURRENCE('Input M3 set screw (1):1',
'Input M3 set screw (1):1','Input M3 set screw (1):1',#27477,#27482,
'Input M3 set screw (1):1');
#492=NEXT_ASSEMBLY_USAGE_OCCURRENCE('Input end keeper:1',
'Input end keeper:1','Input end keeper:1',#27477,#27483,
'Input end keeper:1');
#493=NEXT_ASSEMBLY_USAGE_OCCURRENCE('Motor output shaft:1',
'Motor output shaft:1','Motor output shaft:1',#27477,#27484,
'Motor output shaft:1');
#494=NEXT_ASSEMBLY_USAGE_OCCURRENCE('Motor coupling:1',
'Motor coupling:1','Motor coupling:1',#27477,#27485,'Motor coupling:1');
#495=NEXT_ASSEMBLY_USAGE_OCCURRENCE(
'Timing Pulley - 2 mm Pitch, 20 Teeth, 8 mm Bore:2',
'Timing Pulley - 2 mm Pitch, 20 Teeth, 8 mm Bore:2',
'Timing Pulley - 2 mm Pitch, 20 Teeth, 8 mm Bore:2',#27477,#27486,
'Timing Pulley - 2 mm Pitch, 20 Teeth, 8 mm Bore:2');
#496=NEXT_ASSEMBLY_USAGE_OCCURRENCE('Cap Screw - M4x16:6',
'Cap Screw - M4x16:6','Cap Screw - M4x16:6',#27477,#27502,
'Cap Screw - M4x16:6');
#497=NEXT_ASSEMBLY_USAGE_OCCURRENCE('Socket Set Screw - M5x8:6',
'Socket Set Screw - M5x8:6','Socket Set Screw - M5x8:6',#27477,#27503,
'Socket Set Screw - M5x8:6');
#498=NEXT_ASSEMBLY_USAGE_OCCURRENCE('Socket Set Screw - M5x8:7',
'Socket Set Screw - M5x8:7','Socket Set Screw - M5x8:7',#27477,#27503,
'Socket Set Screw - M5x8:7');
#499=NEXT_ASSEMBLY_USAGE_OCCURRENCE('Output shaft:1','Output shaft:1',
'Output shaft:1',#27487,#27488,'Output shaft:1');
#500=NEXT_ASSEMBLY_USAGE_OCCURRENCE('Output inner spacer:1',
'Output inner spacer:1','Output inner spacer:1',#27487,#27489,
'Output inner spacer:1');
#501=NEXT_ASSEMBLY_USAGE_OCCURRENCE('Output inner sleeve:1',
'Output inner sleeve:1','Output inner sleeve:1',#27487,#27490,
'Output inner sleeve:1');
#502=NEXT_ASSEMBLY_USAGE_OCCURRENCE('Output M3 set screw:1',
'Output M3 set screw:1','Output M3 set screw:1',#27487,#27491,
'Output M3 set screw:1');
#503=NEXT_ASSEMBLY_USAGE_OCCURRENCE('Output M3 set screw (1):1',
'Output M3 set screw (1):1','Output M3 set screw (1):1',#27487,#27492,
'Output M3 set screw (1):1');
#504=NEXT_ASSEMBLY_USAGE_OCCURRENCE('Output end keeper:1',
'Output end keeper:1','Output end keeper:1',#27487,#27493,
'Output end keeper:1');
#505=NEXT_ASSEMBLY_USAGE_OCCURRENCE('Drum shaft collar:1',
'Drum shaft collar:1','Drum shaft collar:1',#27487,#27494,
'Drum shaft collar:1');
#506=NEXT_ASSEMBLY_USAGE_OCCURRENCE('Drum shaft collar (1):1',
'Drum shaft collar (1):1','Drum shaft collar (1):1',#27487,#27495,
'Drum shaft collar (1):1');
#507=NEXT_ASSEMBLY_USAGE_OCCURRENCE('Conveyor drum shell:1',
'Conveyor drum shell:1','Conveyor drum shell:1',#27487,#27496,
'Conveyor drum shell:1');
#508=NEXT_ASSEMBLY_USAGE_OCCURRENCE('Drum end plate:1',
'Drum end plate:1','Drum end plate:1',#27487,#27497,'Drum end plate:1');
#509=NEXT_ASSEMBLY_USAGE_OCCURRENCE('Drum end plate (1):1',
'Drum end plate (1):1','Drum end plate (1):1',#27487,#27498,
'Drum end plate (1):1');
#510=NEXT_ASSEMBLY_USAGE_OCCURRENCE('Drum hub:1','Drum hub:1',
'Drum hub:1',#27487,#27499,'Drum hub:1');
#511=NEXT_ASSEMBLY_USAGE_OCCURRENCE('Drum hub (1):1','Drum hub (1):1',
'Drum hub (1):1',#27487,#27500,'Drum hub (1):1');
#512=NEXT_ASSEMBLY_USAGE_OCCURRENCE(
'Timing Pulley - 2 mm Pitch, 40 Teeth, 12 mm Bore:2',
'Timing Pulley - 2 mm Pitch, 40 Teeth, 12 mm Bore:2',
'Timing Pulley - 2 mm Pitch, 40 Teeth, 12 mm Bore:2',#27487,#27501,
'Timing Pulley - 2 mm Pitch, 40 Teeth, 12 mm Bore:2');
#513=NEXT_ASSEMBLY_USAGE_OCCURRENCE('Cap Screw - M4x16:7',
'Cap Screw - M4x16:7','Cap Screw - M4x16:7',#27487,#27502,
'Cap Screw - M4x16:7');
#514=NEXT_ASSEMBLY_USAGE_OCCURRENCE('Socket Set Screw - M5x8:2',
'Socket Set Screw - M5x8:2','Socket Set Screw - M5x8:2',#27487,#27503,
'Socket Set Screw - M5x8:2');
#515=NEXT_ASSEMBLY_USAGE_OCCURRENCE('Socket Set Screw - M5x8:3',
'Socket Set Screw - M5x8:3','Socket Set Screw - M5x8:3',#27487,#27503,
'Socket Set Screw - M5x8:3');
#516=NEXT_ASSEMBLY_USAGE_OCCURRENCE('Socket Set Screw - M5x8:4',
'Socket Set Screw - M5x8:4','Socket Set Screw - M5x8:4',#27487,#27503,
'Socket Set Screw - M5x8:4');
#517=NEXT_ASSEMBLY_USAGE_OCCURRENCE('Socket Set Screw - M5x8:5',
'Socket Set Screw - M5x8:5','Socket Set Screw - M5x8:5',#27487,#27503,
'Socket Set Screw - M5x8:5');
#518=NEXT_ASSEMBLY_USAGE_OCCURRENCE('Bearing base and belt envelope:1',
'Bearing base and belt envelope:1','Bearing base and belt envelope:1',#27428,
#27429,'Bearing base and belt envelope:1');
#519=NEXT_ASSEMBLY_USAGE_OCCURRENCE('Input pulley and shaft:1',
'Input pulley and shaft:1','Input pulley and shaft:1',#27428,#27477,
'Input pulley and shaft:1');
#520=NEXT_ASSEMBLY_USAGE_OCCURRENCE('Output pulley and shaft:1',
'Output pulley and shaft:1','Output pulley and shaft:1',#27428,#27487,
'Output pulley and shaft:1');
#521=B_SPLINE_CURVE_WITH_KNOTS('',3,(#22504,#22505,#22506,#22507,#22508,
#22509,#22510,#22511,#22512,#22513,#22514,#22515,#22516,#22517,#22518,#22519,
#22520,#22521,#22522,#22523,#22524,#22525),.UNSPECIFIED.,.F.,.F.,(4,2,2,
2,2,2,2,2,2,2,4),(0.0473477652366656,0.126350602536658,0.189525903804987,
0.252701205073317,0.313298422430275,0.373895639787233,0.434492857144191,
0.495090074501149,0.558265375769478,0.621440677037807,0.7004435143378),
 .UNSPECIFIED.);
#522=B_SPLINE_CURVE_WITH_KNOTS('',3,(#22529,#22530,#22531,#22532,#22533,
#22534,#22535,#22536,#22537,#22538,#22539,#22540,#22541,#22542,#22543,#22544,
#22545,#22546,#22547,#22548,#22549,#22550),.UNSPECIFIED.,.F.,.F.,(4,2,2,
2,2,2,2,2,2,2,4),(0.0464897534940957,0.0852567806515119,0.170513561303024,
0.246687263103517,0.308657850341199,0.370628437578881,0.432599024816563,
0.494569612054245,0.570743313854739,0.656000094506251,0.694767121663666),
 .UNSPECIFIED.);
#523=B_SPLINE_CURVE_WITH_KNOTS('',3,(#22556,#22557,#22558,#22559,#22560,
#22561,#22562,#22563,#22564,#22565,#22566,#22567,#22568,#22569,#22570,#22571,
#22572,#22573,#22574,#22575,#22576,#22577),.UNSPECIFIED.,.F.,.F.,(4,2,2,
2,2,2,2,2,2,2,4),(0.0464897534940957,0.0852567806515118,0.170513561303024,
0.246687263103517,0.308657850341199,0.370628437578881,0.432599024816563,
0.494569612054245,0.570743313854738,0.65600009450625,0.694767121663666),
 .UNSPECIFIED.);
#524=B_SPLINE_CURVE_WITH_KNOTS('',3,(#22581,#22582,#22583,#22584,#22585,
#22586,#22587,#22588,#22589,#22590,#22591,#22592,#22593,#22594,#22595,#22596,
#22597,#22598,#22599,#22600,#22601,#22602),.UNSPECIFIED.,.F.,.F.,(4,2,2,
2,2,2,2,2,2,2,4),(0.0464897534940957,0.0852567806515119,0.170513561303024,
0.246687263103517,0.308657850341199,0.370628437578881,0.432599024816563,
0.494569612054245,0.570743313854739,0.656000094506251,0.694767121663666),
 .UNSPECIFIED.);
#525=B_SPLINE_CURVE_WITH_KNOTS('',3,(#22606,#22607,#22608,#22609,#22610,
#22611,#22612,#22613,#22614,#22615,#22616,#22617),.UNSPECIFIED.,.F.,.F.,
(4,2,2,2,2,4),(0.0464897534940957,0.0852567806515119,0.170513561303024,
0.246687263103517,0.308657850341199,0.370628437578881),.UNSPECIFIED.);
#526=B_SPLINE_CURVE_WITH_KNOTS('',3,(#22622,#22623,#22624,#22625,#22626,
#22627,#22628,#22629,#22630,#22631,#22632,#22633),.UNSPECIFIED.,.F.,.F.,
(4,2,2,2,2,4),(0.370628437578881,0.432599024816563,0.494569612054245,0.570743313854738,
0.65600009450625,0.694767121663666),.UNSPECIFIED.);
#527=B_SPLINE_CURVE_WITH_KNOTS('',3,(#22637,#22638,#22639,#22640,#22641,
#22642,#22643,#22644,#22645,#22646,#22647,#22648,#22649,#22650,#22651,#22652,
#22653,#22654,#22655,#22656,#22657,#22658),.UNSPECIFIED.,.F.,.F.,(4,2,2,
2,2,2,2,2,2,2,4),(0.0464897534940957,0.0852567806515121,0.170513561303024,
0.246687263103518,0.308657850341199,0.370628437578881,0.432599024816563,
0.494569612054245,0.570743313854738,0.65600009450625,0.694767121663666),
 .UNSPECIFIED.);
#528=B_SPLINE_CURVE_WITH_KNOTS('',3,(#22662,#22663,#22664,#22665,#22666,
#22667,#22668,#22669,#22670,#22671,#22672,#22673,#22674,#22675,#22676,#22677,
#22678,#22679,#22680,#22681,#22682,#22683),.UNSPECIFIED.,.F.,.F.,(4,2,2,
2,2,2,2,2,2,2,4),(0.0464897534940957,0.0852567806515119,0.170513561303024,
0.246687263103517,0.308657850341199,0.370628437578881,0.432599024816563,
0.494569612054245,0.570743313854738,0.65600009450625,0.694767121663667),
 .UNSPECIFIED.);
#529=B_SPLINE_CURVE_WITH_KNOTS('',3,(#22687,#22688,#22689,#22690,#22691,
#22692,#22693,#22694,#22695,#22696,#22697,#22698,#22699,#22700,#22701,#22702,
#22703,#22704,#22705,#22706,#22707,#22708),.UNSPECIFIED.,.F.,.F.,(4,2,2,
2,2,2,2,2,2,2,4),(0.0464897534940957,0.0852567806515119,0.170513561303024,
0.246687263103517,0.308657850341199,0.370628437578881,0.432599024816563,
0.494569612054245,0.570743313854738,0.65600009450625,0.694767121663666),
 .UNSPECIFIED.);
#530=B_SPLINE_CURVE_WITH_KNOTS('',3,(#22712,#22713,#22714,#22715,#22716,
#22717,#22718,#22719,#22720,#22721,#22722,#22723,#22724,#22725,#22726,#22727,
#22728,#22729,#22730,#22731,#22732,#22733),.UNSPECIFIED.,.F.,.F.,(4,2,2,
2,2,2,2,2,2,2,4),(0.0464897534940957,0.0852567806515119,0.170513561303024,
0.246687263103517,0.308657850341199,0.370628437578881,0.432599024816563,
0.494569612054245,0.570743313854739,0.656000094506251,0.694767121663667),
 .UNSPECIFIED.);
#531=B_SPLINE_CURVE_WITH_KNOTS('',3,(#22741,#22742,#22743,#22744,#22745,
#22746,#22747,#22748,#22749,#22750,#22751,#22752,#22753,#22754,#22755,#22756,
#22757,#22758,#22759,#22760,#22761,#22762),.UNSPECIFIED.,.F.,.F.,(4,2,2,
2,2,2,2,2,2,2,4),(0.0473477652366656,0.126350602536658,0.189525903804987,
0.252701205073316,0.313298422430274,0.373895639787232,0.434492857144191,
0.495090074501149,0.558265375769478,0.621440677037807,0.7004435143378),
 .UNSPECIFIED.);
#532=B_SPLINE_CURVE_WITH_KNOTS('',3,(#22770,#22771,#22772,#22773,#22774,
#22775,#22776,#22777,#22778,#22779,#22780,#22781,#22782,#22783,#22784,#22785,
#22786,#22787,#22788,#22789,#22790,#22791),.UNSPECIFIED.,.F.,.F.,(4,2,2,
2,2,2,2,2,2,2,4),(0.0473477652366656,0.126350602536658,0.189525903804987,
0.252701205073317,0.313298422430275,0.373895639787233,0.434492857144191,
0.495090074501149,0.558265375769478,0.621440677037807,0.7004435143378),
 .UNSPECIFIED.);
#533=B_SPLINE_CURVE_WITH_KNOTS('',3,(#22800,#22801,#22802,#22803,#22804,
#22805,#22806,#22807,#22808,#22809,#22810,#22811),.UNSPECIFIED.,.F.,.F.,
(4,2,2,2,2,4),(0.0473477652366656,0.126350602536658,0.189525903804987,0.252701205073316,
0.313298422430275,0.373895639787233),.UNSPECIFIED.);
#534=B_SPLINE_CURVE_WITH_KNOTS('',3,(#22813,#22814,#22815,#22816,#22817,
#22818,#22819,#22820,#22821,#22822,#22823,#22824),.UNSPECIFIED.,.F.,.F.,
(4,2,2,2,2,4),(0.373895639787233,0.434492857144191,0.495090074501149,0.558265375769478,
0.621440677037807,0.7004435143378),.UNSPECIFIED.);
#535=B_SPLINE_CURVE_WITH_KNOTS('',3,(#22831,#22832,#22833,#22834,#22835,
#22836,#22837,#22838,#22839,#22840,#22841,#22842,#22843,#22844,#22845,#22846,
#22847,#22848,#22849,#22850,#22851,#22852),.UNSPECIFIED.,.F.,.F.,(4,2,2,
2,2,2,2,2,2,2,4),(0.0473477652366656,0.126350602536658,0.189525903804987,
0.252701205073316,0.313298422430275,0.373895639787233,0.434492857144191,
0.495090074501149,0.558265375769478,0.621440677037807,0.7004435143378),
 .UNSPECIFIED.);
#536=B_SPLINE_CURVE_WITH_KNOTS('',3,(#22860,#22861,#22862,#22863,#22864,
#22865,#22866,#22867,#22868,#22869,#22870,#22871,#22872,#22873,#22874,#22875,
#22876,#22877,#22878,#22879,#22880,#22881),.UNSPECIFIED.,.F.,.F.,(4,2,2,
2,2,2,2,2,2,2,4),(0.0473477652366656,0.126350602536658,0.189525903804987,
0.252701205073317,0.313298422430275,0.373895639787233,0.434492857144191,
0.495090074501149,0.558265375769478,0.621440677037807,0.7004435143378),
 .UNSPECIFIED.);
#537=B_SPLINE_CURVE_WITH_KNOTS('',3,(#22889,#22890,#22891,#22892,#22893,
#22894,#22895,#22896,#22897,#22898,#22899,#22900,#22901,#22902,#22903,#22904,
#22905,#22906,#22907,#22908,#22909,#22910),.UNSPECIFIED.,.F.,.F.,(4,2,2,
2,2,2,2,2,2,2,4),(0.0473477652366656,0.126350602536658,0.189525903804987,
0.252701205073316,0.313298422430275,0.373895639787233,0.434492857144191,
0.495090074501149,0.558265375769478,0.621440677037807,0.7004435143378),
 .UNSPECIFIED.);
#538=B_SPLINE_CURVE_WITH_KNOTS('',3,(#22919,#22920,#22921,#22922,#22923,
#22924,#22925,#22926,#22927,#22928,#22929,#22930,#22931,#22932,#22933,#22934,
#22935,#22936,#22937,#22938,#22939,#22940),.UNSPECIFIED.,.F.,.F.,(4,2,2,
2,2,2,2,2,2,2,4),(0.0473477652366656,0.126350602536658,0.189525903804987,
0.252701205073317,0.313298422430275,0.373895639787233,0.434492857144191,
0.495090074501149,0.558265375769478,0.621440677037807,0.7004435143378),
 .UNSPECIFIED.);
#539=B_SPLINE_CURVE_WITH_KNOTS('',3,(#23163,#23164,#23165,#23166,#23167,
#23168,#23169,#23170,#23171,#23172,#23173,#23174,#23175,#23176,#23177,#23178,
#23179,#23180,#23181,#23182,#23183,#23184),.UNSPECIFIED.,.F.,.F.,(4,2,2,
2,2,2,2,2,2,2,4),(0.0591825211272536,0.157966726598481,0.236950089897721,
0.315933453196962,0.391576304923761,0.46721915665056,0.54286200837736,0.618504860104159,
0.697488223403399,0.77647158670264,0.875255792173867),.UNSPECIFIED.);
#540=B_SPLINE_CURVE_WITH_KNOTS('',3,(#23188,#23189,#23190,#23191,#23192,
#23193,#23194,#23195,#23196,#23197,#23198,#23199,#23200,#23201,#23202,#23203,
#23204,#23205,#23206,#23207,#23208,#23209),.UNSPECIFIED.,.F.,.F.,(4,2,2,
2,2,2,2,2,2,2,4),(0.0581119756758434,0.106553146291161,0.213106292582322,
0.30849933801665,0.386091982889075,0.4636846277615,0.541277272633925,0.61886991750635,
0.714262962940678,0.820816109231839,0.869257279847157),.UNSPECIFIED.);
#541=B_SPLINE_CURVE_WITH_KNOTS('',3,(#23215,#23216,#23217,#23218,#23219,
#23220,#23221,#23222,#23223,#23224,#23225,#23226,#23227,#23228,#23229,#23230,
#23231,#23232,#23233,#23234,#23235,#23236),.UNSPECIFIED.,.F.,.F.,(4,2,2,
2,2,2,2,2,2,2,4),(0.0581119756758434,0.106553146291161,0.213106292582322,
0.30849933801665,0.386091982889075,0.4636846277615,0.541277272633925,0.61886991750635,
0.714262962940679,0.820816109231839,0.869257279847157),.UNSPECIFIED.);
#542=B_SPLINE_CURVE_WITH_KNOTS('',3,(#23240,#23241,#23242,#23243,#23244,
#23245,#23246,#23247,#23248,#23249,#23250,#23251,#23252,#23253,#23254,#23255,
#23256,#23257,#23258,#23259,#23260,#23261),.UNSPECIFIED.,.F.,.F.,(4,2,2,
2,2,2,2,2,2,2,4),(0.0581119756758433,0.106553146291161,0.213106292582322,
0.308499338016649,0.386091982889075,0.4636846277615,0.541277272633925,0.61886991750635,
0.714262962940678,0.820816109231839,0.869257279847157),.UNSPECIFIED.);
#543=B_SPLINE_CURVE_WITH_KNOTS('',3,(#23270,#23271,#23272,#23273,#23274,
#23275,#23276,#23277,#23278,#23279,#23280,#23281,#23282,#23283,#23284,#23285,
#23286,#23287,#23288,#23289,#23290,#23291),.UNSPECIFIED.,.F.,.F.,(4,2,2,
2,2,2,2,2,2,2,4),(0.0581119756758433,0.106553146291161,0.213106292582322,
0.30849933801665,0.386091982889075,0.4636846277615,0.541277272633925,0.61886991750635,
0.714262962940678,0.820816109231839,0.869257279847157),.UNSPECIFIED.);
#544=B_SPLINE_CURVE_WITH_KNOTS('',3,(#23295,#23296,#23297,#23298,#23299,
#23300,#23301,#23302,#23303,#23304,#23305,#23306,#23307,#23308,#23309,#23310,
#23311,#23312,#23313,#23314,#23315,#23316),.UNSPECIFIED.,.F.,.F.,(4,2,2,
2,2,2,2,2,2,2,4),(0.0581119756758434,0.106553146291161,0.213106292582322,
0.30849933801665,0.386091982889075,0.4636846277615,0.541277272633925,0.61886991750635,
0.714262962940678,0.820816109231839,0.869257279847157),.UNSPECIFIED.);
#545=B_SPLINE_CURVE_WITH_KNOTS('',3,(#23320,#23321,#23322,#23323,#23324,
#23325,#23326,#23327,#23328,#23329,#23330,#23331,#23332,#23333,#23334,#23335,
#23336,#23337,#23338,#23339,#23340,#23341),.UNSPECIFIED.,.F.,.F.,(4,2,2,
2,2,2,2,2,2,2,4),(0.0581119756758434,0.106553146291161,0.213106292582322,
0.30849933801665,0.386091982889075,0.4636846277615,0.541277272633925,0.61886991750635,
0.714262962940678,0.820816109231839,0.869257279847157),.UNSPECIFIED.);
#546=B_SPLINE_CURVE_WITH_KNOTS('',3,(#23345,#23346,#23347,#23348,#23349,
#23350,#23351,#23352,#23353,#23354,#23355,#23356,#23357,#23358,#23359,#23360,
#23361,#23362,#23363,#23364,#23365,#23366),.UNSPECIFIED.,.F.,.F.,(4,2,2,
2,2,2,2,2,2,2,4),(0.0581119756758433,0.106553146291161,0.213106292582322,
0.30849933801665,0.386091982889075,0.4636846277615,0.541277272633925,0.61886991750635,
0.714262962940678,0.820816109231839,0.869257279847157),.UNSPECIFIED.);
#547=B_SPLINE_CURVE_WITH_KNOTS('',3,(#23374,#23375,#23376,#23377,#23378,
#23379,#23380,#23381,#23382,#23383,#23384,#23385,#23386,#23387,#23388,#23389,
#23390,#23391,#23392,#23393,#23394,#23395),.UNSPECIFIED.,.F.,.F.,(4,2,2,
2,2,2,2,2,2,2,4),(0.0591825211272536,0.157966726598481,0.236950089897721,
0.315933453196962,0.391576304923761,0.467219156650561,0.54286200837736,
0.618504860104159,0.697488223403399,0.77647158670264,0.875255792173867),
 .UNSPECIFIED.);
#548=B_SPLINE_CURVE_WITH_KNOTS('',3,(#23403,#23404,#23405,#23406,#23407,
#23408,#23409,#23410,#23411,#23412,#23413,#23414,#23415,#23416,#23417,#23418,
#23419,#23420,#23421,#23422,#23423,#23424),.UNSPECIFIED.,.F.,.F.,(4,2,2,
2,2,2,2,2,2,2,4),(0.0591825211272536,0.157966726598481,0.236950089897722,
0.315933453196962,0.391576304923761,0.467219156650561,0.54286200837736,
0.618504860104159,0.697488223403399,0.77647158670264,0.875255792173867),
 .UNSPECIFIED.);
#549=B_SPLINE_CURVE_WITH_KNOTS('',3,(#23434,#23435,#23436,#23437,#23438,
#23439,#23440,#23441,#23442,#23443,#23444,#23445,#23446,#23447,#23448,#23449,
#23450,#23451,#23452,#23453,#23454,#23455),.UNSPECIFIED.,.F.,.F.,(4,2,2,
2,2,2,2,2,2,2,4),(0.0591825211272536,0.157966726598481,0.236950089897721,
0.315933453196962,0.391576304923761,0.46721915665056,0.54286200837736,0.618504860104159,
0.697488223403399,0.77647158670264,0.875255792173867),.UNSPECIFIED.);
#550=B_SPLINE_CURVE_WITH_KNOTS('',3,(#23463,#23464,#23465,#23466,#23467,
#23468,#23469,#23470,#23471,#23472,#23473,#23474,#23475,#23476,#23477,#23478,
#23479,#23480,#23481,#23482,#23483,#23484),.UNSPECIFIED.,.F.,.F.,(4,2,2,
2,2,2,2,2,2,2,4),(0.0591825211272536,0.157966726598481,0.236950089897721,
0.315933453196962,0.391576304923761,0.46721915665056,0.542862008377359,
0.618504860104159,0.697488223403399,0.776471586702639,0.875255792173867),
 .UNSPECIFIED.);
#551=B_SPLINE_CURVE_WITH_KNOTS('',3,(#23492,#23493,#23494,#23495,#23496,
#23497,#23498,#23499,#23500,#23501,#23502,#23503,#23504,#23505,#23506,#23507,
#23508,#23509,#23510,#23511,#23512,#23513),.UNSPECIFIED.,.F.,.F.,(4,2,2,
2,2,2,2,2,2,2,4),(0.0591825211272536,0.157966726598481,0.236950089897721,
0.315933453196962,0.391576304923761,0.46721915665056,0.54286200837736,0.618504860104159,
0.697488223403399,0.77647158670264,0.875255792173867),.UNSPECIFIED.);
#552=B_SPLINE_CURVE_WITH_KNOTS('',3,(#23522,#23523,#23524,#23525,#23526,
#23527,#23528,#23529,#23530,#23531,#23532,#23533,#23534,#23535,#23536,#23537,
#23538,#23539,#23540,#23541,#23542,#23543),.UNSPECIFIED.,.F.,.F.,(4,2,2,
2,2,2,2,2,2,2,4),(0.0591825211272536,0.157966726598481,0.236950089897721,
0.315933453196962,0.391576304923761,0.46721915665056,0.542862008377359,
0.618504860104159,0.697488223403399,0.776471586702639,0.875255792173867),
 .UNSPECIFIED.);
#553=B_SPLINE_CURVE_WITH_KNOTS('',3,(#23805,#23806,#23807,#23808,#23809,
#23810,#23811,#23812,#23813,#23814),.UNSPECIFIED.,.F.,.F.,(4,2,2,2,4),(1.13193471301885,
1.22626174930539,1.32058878559194,1.41491753480854,1.50924628402513),
 .UNSPECIFIED.);
#554=B_SPLINE_CURVE_WITH_KNOTS('',3,(#23816,#23817,#23818,#23819,#23820,
#23821,#23822,#23823,#23824,#23825,#23826,#23827,#23828,#23829,#23830,#23831,
#23832,#23833),.UNSPECIFIED.,.F.,.F.,(4,2,2,2,2,2,2,2,4),(0.377311571006283,
0.471638607292829,0.565965643579376,0.66029439279597,0.754623142012565,
0.84895189122916,0.943280640445754,1.0376076767323,1.13193471301885),
 .UNSPECIFIED.);
#555=B_SPLINE_CURVE_WITH_KNOTS('',3,(#23834,#23835,#23836,#23837,#23838,
#23839,#23840,#23841,#23842,#23843),.UNSPECIFIED.,.F.,.F.,(4,2,2,2,4),(1.50924628402513,
1.60357503324173,1.69790378245832,1.79223081874487,1.88655785503141),
 .UNSPECIFIED.);
#556=B_SPLINE_CURVE_WITH_KNOTS('',3,(#23846,#23847,#23848,#23849,#23850,
#23851,#23852,#23853,#23854,#23855,#23856,#23857,#23858,#23859,#23860,#23861,
#23862,#23863,#23864,#23865,#23866,#23867,#23868,#23869,#23870,#23871,#23872,
#23873,#23874,#23875,#23876,#23877,#23878,#23879),.UNSPECIFIED.,.T.,.F.,
(4,2,2,2,2,2,2,2,2,2,2,2,2,2,2,2,4),(0.,0.0946120580087934,0.189224116017587,
0.283822945575014,0.378421775132442,0.47302060468987,0.567619434247297,
0.662231492256091,0.756843550264884,0.851455608273677,0.94606766628247,
1.0406664958399,1.13526532539733,1.22986415495475,1.32446298451218,1.41907504252097,
1.51368710052977),.UNSPECIFIED.);
#557=B_SPLINE_CURVE_WITH_KNOTS('',3,(#23882,#23883,#23884,#23885,#23886,
#23887,#23888,#23889,#23890,#23891,#23892,#23893,#23894,#23895,#23896,#23897,
#23898,#23899,#23900,#23901,#23902,#23903,#23904,#23905,#23906,#23907,#23908,
#23909,#23910,#23911,#23912,#23913,#23914,#23915),.UNSPECIFIED.,.T.,.F.,
(4,2,2,2,2,2,2,2,2,2,2,2,2,2,2,2,4),(0.,0.0946120580087934,0.189224116017587,
0.283822945575014,0.378421775132442,0.47302060468987,0.567619434247297,
0.66223149225609,0.756843550264884,0.851455608273677,0.94606766628247,1.0406664958399,
1.13526532539733,1.22986415495475,1.32446298451218,1.41907504252097,1.51368710052977),
 .UNSPECIFIED.);
#558=B_SPLINE_CURVE_WITH_KNOTS('',3,(#23919,#23920,#23921,#23922,#23923,
#23924,#23925,#23926,#23927,#23928),.UNSPECIFIED.,.F.,.F.,(4,2,2,2,4),(1.13193471301885,
1.22626174930539,1.32058878559194,1.41491753480854,1.50924628402513),
 .UNSPECIFIED.);
#559=B_SPLINE_CURVE_WITH_KNOTS('',3,(#23930,#23931,#23932,#23933,#23934,
#23935,#23936,#23937,#23938,#23939,#23940,#23941,#23942,#23943,#23944,#23945,
#23946,#23947),.UNSPECIFIED.,.F.,.F.,(4,2,2,2,2,2,2,2,4),(0.377311571006283,
0.47163860729283,0.565965643579376,0.660294392795971,0.754623142012565,
0.84895189122916,0.943280640445755,1.0376076767323,1.13193471301885),
 .UNSPECIFIED.);
#560=B_SPLINE_CURVE_WITH_KNOTS('',3,(#23948,#23949,#23950,#23951,#23952,
#23953,#23954,#23955,#23956,#23957),.UNSPECIFIED.,.F.,.F.,(4,2,2,2,4),(1.50924628402513,
1.60357503324173,1.69790378245832,1.79223081874487,1.88655785503141),
 .UNSPECIFIED.);
#561=B_SPLINE_CURVE_WITH_KNOTS('',3,(#23966,#23967,#23968,#23969,#23970,
#23971,#23972,#23973,#23974,#23975,#23976,#23977,#23978,#23979,#23980,#23981,
#23982,#23983),.UNSPECIFIED.,.F.,.F.,(4,2,2,2,2,2,2,2,4),(0.377311571006282,
0.471638607292829,0.565965643579376,0.660294392795971,0.754623142012565,
0.84895189122916,0.943280640445754,1.0376076767323,1.13193471301885),
 .UNSPECIFIED.);
#562=B_SPLINE_CURVE_WITH_KNOTS('',3,(#23985,#23986,#23987,#23988,#23989,
#23990,#23991,#23992,#23993,#23994),.UNSPECIFIED.,.F.,.F.,(4,2,2,2,4),(1.13193471301885,
1.22626174930539,1.32058878559194,1.41491753480854,1.50924628402513),
 .UNSPECIFIED.);
#563=B_SPLINE_CURVE_WITH_KNOTS('',3,(#23995,#23996,#23997,#23998,#23999,
#24000,#24001,#24002,#24003,#24004),.UNSPECIFIED.,.F.,.F.,(4,2,2,2,4),(1.50924628402513,
1.60357503324172,1.69790378245832,1.79223081874487,1.88655785503141),
 .UNSPECIFIED.);
#564=B_SPLINE_CURVE_WITH_KNOTS('',3,(#24007,#24008,#24009,#24010,#24011,
#24012,#24013,#24014,#24015,#24016,#24017,#24018,#24019,#24020,#24021,#24022,
#24023,#24024),.UNSPECIFIED.,.F.,.F.,(4,2,2,2,2,2,2,2,4),(0.377311571006283,
0.47163860729283,0.565965643579376,0.660294392795971,0.754623142012565,
0.84895189122916,0.943280640445754,1.0376076767323,1.13193471301885),
 .UNSPECIFIED.);
#565=B_SPLINE_CURVE_WITH_KNOTS('',3,(#24026,#24027,#24028,#24029,#24030,
#24031,#24032,#24033,#24034,#24035),.UNSPECIFIED.,.F.,.F.,(4,2,2,2,4),(1.13193471301885,
1.22626174930539,1.32058878559194,1.41491753480854,1.50924628402513),
 .UNSPECIFIED.);
#566=B_SPLINE_CURVE_WITH_KNOTS('',3,(#24036,#24037,#24038,#24039,#24040,
#24041,#24042,#24043,#24044,#24045),.UNSPECIFIED.,.F.,.F.,(4,2,2,2,4),(1.50924628402513,
1.60357503324173,1.69790378245832,1.79223081874487,1.88655785503141),
 .UNSPECIFIED.);
#567=B_SPLINE_CURVE_WITH_KNOTS('',3,(#24048,#24049,#24050,#24051,#24052,
#24053,#24054,#24055,#24056,#24057,#24058,#24059,#24060,#24061,#24062,#24063,
#24064,#24065),.UNSPECIFIED.,.F.,.F.,(4,2,2,2,2,2,2,2,4),(0.377311571006282,
0.471638607292829,0.565965643579376,0.66029439279597,0.754623142012565,
0.84895189122916,0.943280640445754,1.0376076767323,1.13193471301885),
 .UNSPECIFIED.);
#568=B_SPLINE_CURVE_WITH_KNOTS('',3,(#24067,#24068,#24069,#24070,#24071,
#24072,#24073,#24074,#24075,#24076),.UNSPECIFIED.,.F.,.F.,(4,2,2,2,4),(1.13193471301885,
1.22626174930539,1.32058878559194,1.41491753480854,1.50924628402513),
 .UNSPECIFIED.);
#569=B_SPLINE_CURVE_WITH_KNOTS('',3,(#24077,#24078,#24079,#24080,#24081,
#24082,#24083,#24084,#24085,#24086),.UNSPECIFIED.,.F.,.F.,(4,2,2,2,4),(1.50924628402513,
1.60357503324172,1.69790378245832,1.79223081874487,1.88655785503141),
 .UNSPECIFIED.);
#570=B_SPLINE_CURVE_WITH_KNOTS('',3,(#24089,#24090,#24091,#24092,#24093,
#24094,#24095,#24096,#24097,#24098,#24099,#24100,#24101,#24102,#24103,#24104,
#24105,#24106),.UNSPECIFIED.,.F.,.F.,(4,2,2,2,2,2,2,2,4),(0.377311571006283,
0.471638607292829,0.565965643579376,0.660294392795971,0.754623142012565,
0.84895189122916,0.943280640445755,1.0376076767323,1.13193471301885),
 .UNSPECIFIED.);
#571=B_SPLINE_CURVE_WITH_KNOTS('',3,(#24108,#24109,#24110,#24111,#24112,
#24113,#24114,#24115,#24116,#24117),.UNSPECIFIED.,.F.,.F.,(4,2,2,2,4),(1.13193471301885,
1.22626174930539,1.32058878559194,1.41491753480854,1.50924628402513),
 .UNSPECIFIED.);
#572=B_SPLINE_CURVE_WITH_KNOTS('',3,(#24118,#24119,#24120,#24121,#24122,
#24123,#24124,#24125,#24126,#24127),.UNSPECIFIED.,.F.,.F.,(4,2,2,2,4),(1.50924628402513,
1.60357503324172,1.69790378245832,1.79223081874487,1.88655785503141),
 .UNSPECIFIED.);
#573=B_SPLINE_CURVE_WITH_KNOTS('',3,(#24131,#24132,#24133,#24134,#24135,
#24136,#24137,#24138,#24139,#24140,#24141,#24142,#24143,#24144,#24145,#24146,
#24147,#24148,#24149,#24150,#24151,#24152,#24153,#24154,#24155,#24156,#24157,
#24158,#24159,#24160,#24161,#24162,#24163,#24164),.UNSPECIFIED.,.T.,.F.,
(4,2,2,2,2,2,2,2,2,2,2,2,2,2,2,2,4),(0.,0.0946120580087934,0.189224116017587,
0.283822945575014,0.378421775132442,0.47302060468987,0.567619434247297,
0.66223149225609,0.756843550264884,0.851455608273677,0.94606766628247,1.0406664958399,
1.13526532539733,1.22986415495475,1.32446298451218,1.41907504252097,1.51368710052977),
 .UNSPECIFIED.);
#574=B_SPLINE_CURVE_WITH_KNOTS('',3,(#24167,#24168,#24169,#24170,#24171,
#24172,#24173,#24174,#24175,#24176,#24177,#24178,#24179,#24180,#24181,#24182,
#24183,#24184,#24185,#24186,#24187,#24188,#24189,#24190,#24191,#24192,#24193,
#24194,#24195,#24196,#24197,#24198,#24199,#24200),.UNSPECIFIED.,.T.,.F.,
(4,2,2,2,2,2,2,2,2,2,2,2,2,2,2,2,4),(0.,0.0946120580087934,0.189224116017587,
0.283822945575014,0.378421775132442,0.47302060468987,0.567619434247297,
0.66223149225609,0.756843550264884,0.851455608273677,0.94606766628247,1.0406664958399,
1.13526532539733,1.22986415495475,1.32446298451218,1.41907504252097,1.51368710052977),
 .UNSPECIFIED.);
#575=B_SPLINE_CURVE_WITH_KNOTS('',3,(#24205,#24206,#24207,#24208,#24209,
#24210,#24211,#24212,#24213,#24214,#24215,#24216,#24217,#24218,#24219,#24220,
#24221,#24222,#24223,#24224,#24225,#24226,#24227,#24228,#24229,#24230,#24231,
#24232,#24233,#24234,#24235,#24236,#24237,#24238),.UNSPECIFIED.,.T.,.F.,
(4,2,2,2,2,2,2,2,2,2,2,2,2,2,2,2,4),(0.,0.0946120580087934,0.189224116017587,
0.283822945575014,0.378421775132442,0.47302060468987,0.567619434247297,
0.66223149225609,0.756843550264884,0.851455608273677,0.94606766628247,1.0406664958399,
1.13526532539733,1.22986415495475,1.32446298451218,1.41907504252097,1.51368710052977),
 .UNSPECIFIED.);
#576=B_SPLINE_CURVE_WITH_KNOTS('',3,(#24241,#24242,#24243,#24244,#24245,
#24246,#24247,#24248,#24249,#24250,#24251,#24252,#24253,#24254,#24255,#24256,
#24257,#24258,#24259,#24260,#24261,#24262,#24263,#24264,#24265,#24266,#24267,
#24268,#24269,#24270,#24271,#24272,#24273,#24274),.UNSPECIFIED.,.T.,.F.,
(4,2,2,2,2,2,2,2,2,2,2,2,2,2,2,2,4),(0.,0.0946120580087934,0.189224116017587,
0.283822945575014,0.378421775132442,0.47302060468987,0.567619434247297,
0.66223149225609,0.756843550264884,0.851455608273677,0.94606766628247,1.0406664958399,
1.13526532539733,1.22986415495475,1.32446298451218,1.41907504252097,1.51368710052977),
 .UNSPECIFIED.);
#577=B_SPLINE_CURVE_WITH_KNOTS('',3,(#24565,#24566,#24567,#24568,#24569,
#24570,#24571,#24572,#24573,#24574),.UNSPECIFIED.,.F.,.F.,(4,2,2,2,4),(0.83629428206811,
0.881958251377254,0.962083854030852,1.04220945668445,1.08787342599359),
 .UNSPECIFIED.);
#578=B_SPLINE_CURVE_WITH_KNOTS('',3,(#24580,#24581,#24582,#24583,#24584,
#24585,#24586,#24587,#24588,#24589,#24590,#24591,#24592,#24593,#24594,#24595,
#24596,#24597),.UNSPECIFIED.,.F.,.F.,(4,2,2,2,2,2,2,2,4),(0.,0.0793616477694785,
0.158723295538957,0.238079516586307,0.317435737633656,0.396791958681006,
0.476148179728355,0.555509827497834,0.634871475267312),.UNSPECIFIED.);
#579=B_SPLINE_CURVE_WITH_KNOTS('',3,(#24598,#24599,#24600,#24601,#24602,
#24603,#24604,#24605,#24606,#24607,#24608,#24609,#24610,#24611,#24612,#24613,
#24614,#24615),.UNSPECIFIED.,.F.,.F.,(4,2,2,2,2,2,2,2,4),(0.634871475267312,
0.714233123036791,0.793594770806269,0.872950991853619,0.952307212900968,
1.03166343394832,1.11101965499567,1.19038130276515,1.26974295053462),
 .UNSPECIFIED.);
#580=B_SPLINE_CURVE_WITH_KNOTS('',3,(#24618,#24619,#24620,#24621,#24622,
#24623,#24624,#24625,#24626,#24627),.UNSPECIFIED.,.F.,.F.,(4,2,2,2,4),(0.194905046047542,
0.240569015356686,0.320694618010284,0.400820220663882,0.446484189973025),
 .UNSPECIFIED.);
#581=B_SPLINE_CURVE_WITH_KNOTS('',3,(#24637,#24638,#24639,#24640,#24641,
#24642,#24643,#24644,#24645,#24646),.UNSPECIFIED.,.F.,.F.,(4,2,2,2,4),(0.83629428206811,
0.881958251377254,0.962083854030852,1.04220945668445,1.08787342599359),
 .UNSPECIFIED.);
#582=B_SPLINE_CURVE_WITH_KNOTS('',3,(#24652,#24653,#24654,#24655,#24656,
#24657,#24658,#24659,#24660,#24661,#24662,#24663,#24664,#24665,#24666,#24667,
#24668,#24669),.UNSPECIFIED.,.F.,.F.,(4,2,2,2,2,2,2,2,4),(0.,0.0793616477694785,
0.158723295538957,0.238079516586307,0.317435737633656,0.396791958681006,
0.476148179728355,0.555509827497834,0.634871475267312),.UNSPECIFIED.);
#583=B_SPLINE_CURVE_WITH_KNOTS('',3,(#24670,#24671,#24672,#24673,#24674,
#24675,#24676,#24677,#24678,#24679,#24680,#24681,#24682,#24683,#24684,#24685,
#24686,#24687),.UNSPECIFIED.,.F.,.F.,(4,2,2,2,2,2,2,2,4),(0.634871475267312,
0.714233123036791,0.793594770806269,0.872950991853619,0.952307212900968,
1.03166343394832,1.11101965499567,1.19038130276515,1.26974295053462),
 .UNSPECIFIED.);
#584=B_SPLINE_CURVE_WITH_KNOTS('',3,(#24690,#24691,#24692,#24693,#24694,
#24695,#24696,#24697,#24698,#24699),.UNSPECIFIED.,.F.,.F.,(4,2,2,2,4),(0.194905046047542,
0.240569015356686,0.320694618010284,0.400820220663882,0.446484189973025),
 .UNSPECIFIED.);
#585=B_SPLINE_CURVE_WITH_KNOTS('',3,(#24720,#24721,#24722,#24723,#24724,
#24725,#24726,#24727,#24728,#24729),.UNSPECIFIED.,.F.,.F.,(4,2,2,2,4),(0.566550474129931,
0.613761886174531,0.66097329821913,0.708186965196186,0.755400632173242),
 .UNSPECIFIED.);
#586=B_SPLINE_CURVE_WITH_KNOTS('',3,(#24731,#24732,#24733,#24734,#24735,
#24736,#24737,#24738,#24739,#24740,#24741,#24742,#24743,#24744,#24745,#24746,
#24747,#24748),.UNSPECIFIED.,.F.,.F.,(4,2,2,2,2,2,2,2,4),(0.18885015804331,
0.23606157008791,0.283272982132509,0.330486649109565,0.377700316086621,
0.424913983063677,0.472127650040732,0.519339062085332,0.566550474129931),
 .UNSPECIFIED.);
#587=B_SPLINE_CURVE_WITH_KNOTS('',3,(#24749,#24750,#24751,#24752,#24753,
#24754,#24755,#24756,#24757,#24758),.UNSPECIFIED.,.F.,.F.,(4,2,2,2,4),(0.755400632173242,
0.802614299150298,0.849827966127353,0.897039378171953,0.944250790216552),
 .UNSPECIFIED.);
#588=B_SPLINE_CURVE_WITH_KNOTS('',3,(#24762,#24763,#24764,#24765,#24766,
#24767,#24768,#24769,#24770,#24771),.UNSPECIFIED.,.F.,.F.,(4,2,2,2,4),(0.189723673274825,
0.237146208024627,0.28456874277443,0.33200804466204,0.37944734654965),
 .UNSPECIFIED.);
#589=B_SPLINE_CURVE_WITH_KNOTS('',3,(#24773,#24774,#24775,#24776,#24777,
#24778,#24779,#24780,#24781,#24782),.UNSPECIFIED.,.F.,.F.,(4,2,2,2,4),(0.,
0.0474393018876097,0.0948786037752193,0.142301138525022,0.189723673274825),
 .UNSPECIFIED.);
#590=B_SPLINE_CURVE_WITH_KNOTS('',3,(#24784,#24785,#24786,#24787,#24788,
#24789,#24790,#24791,#24792,#24793),.UNSPECIFIED.,.F.,.F.,(4,2,2,2,4),(0.569171019824474,
0.616593554574277,0.66401608932408,0.711455391211689,0.758894693099299),
 .UNSPECIFIED.);
#591=B_SPLINE_CURVE_WITH_KNOTS('',3,(#24794,#24795,#24796,#24797,#24798,
#24799,#24800,#24801,#24802,#24803),.UNSPECIFIED.,.F.,.F.,(4,2,2,2,4),(0.37944734654965,
0.426886648437259,0.474325950324869,0.521748485074671,0.569171019824474),
 .UNSPECIFIED.);
#592=B_SPLINE_CURVE_WITH_KNOTS('',3,(#24807,#24808,#24809,#24810,#24811,
#24812,#24813,#24814,#24815,#24816,#24817,#24818,#24819,#24820,#24821,#24822,
#24823,#24824),.UNSPECIFIED.,.F.,.F.,(4,2,2,2,2,2,2,2,4),(0.,0.0474393018876097,
0.0948786037752194,0.142301138525022,0.189723673274825,0.237146208024628,
0.28456874277443,0.33200804466204,0.37944734654965),.UNSPECIFIED.);
#593=B_SPLINE_CURVE_WITH_KNOTS('',3,(#24825,#24826,#24827,#24828,#24829,
#24830,#24831,#24832,#24833,#24834,#24835,#24836,#24837,#24838,#24839,#24840,
#24841,#24842),.UNSPECIFIED.,.F.,.F.,(4,2,2,2,2,2,2,2,4),(0.37944734654965,
0.426886648437259,0.474325950324869,0.521748485074672,0.569171019824474,
0.616593554574277,0.66401608932408,0.711455391211689,0.758894693099299),
 .UNSPECIFIED.);
#594=B_SPLINE_CURVE_WITH_KNOTS('',3,(#24846,#24847,#24848,#24849,#24850,
#24851,#24852,#24853,#24854,#24855),.UNSPECIFIED.,.F.,.F.,(4,2,2,2,4),(0.566550474129931,
0.613761886174531,0.66097329821913,0.708186965196186,0.755400632173242),
 .UNSPECIFIED.);
#595=B_SPLINE_CURVE_WITH_KNOTS('',3,(#24857,#24858,#24859,#24860,#24861,
#24862,#24863,#24864,#24865,#24866,#24867,#24868,#24869,#24870,#24871,#24872,
#24873,#24874),.UNSPECIFIED.,.F.,.F.,(4,2,2,2,2,2,2,2,4),(0.188850158043311,
0.23606157008791,0.283272982132509,0.330486649109565,0.377700316086621,
0.424913983063677,0.472127650040733,0.519339062085332,0.566550474129931),
 .UNSPECIFIED.);
#596=B_SPLINE_CURVE_WITH_KNOTS('',3,(#24875,#24876,#24877,#24878,#24879,
#24880,#24881,#24882,#24883,#24884),.UNSPECIFIED.,.F.,.F.,(4,2,2,2,4),(0.755400632173242,
0.802614299150298,0.849827966127354,0.897039378171953,0.944250790216552),
 .UNSPECIFIED.);
#597=B_SPLINE_CURVE_WITH_KNOTS('',3,(#24894,#24895,#24896,#24897,#24898,
#24899,#24900,#24901,#24902,#24903,#24904,#24905,#24906,#24907,#24908,#24909,
#24910,#24911),.UNSPECIFIED.,.F.,.F.,(4,2,2,2,2,2,2,2,4),(0.18885015804331,
0.23606157008791,0.283272982132509,0.330486649109565,0.377700316086621,
0.424913983063677,0.472127650040732,0.519339062085332,0.566550474129931),
 .UNSPECIFIED.);
#598=B_SPLINE_CURVE_WITH_KNOTS('',3,(#24913,#24914,#24915,#24916,#24917,
#24918,#24919,#24920,#24921,#24922),.UNSPECIFIED.,.F.,.F.,(4,2,2,2,4),(0.566550474129931,
0.613761886174531,0.66097329821913,0.708186965196186,0.755400632173242),
 .UNSPECIFIED.);
#599=B_SPLINE_CURVE_WITH_KNOTS('',3,(#24923,#24924,#24925,#24926,#24927,
#24928,#24929,#24930,#24931,#24932),.UNSPECIFIED.,.F.,.F.,(4,2,2,2,4),(0.755400632173242,
0.802614299150298,0.849827966127353,0.897039378171953,0.944250790216552),
 .UNSPECIFIED.);
#600=B_SPLINE_CURVE_WITH_KNOTS('',3,(#24935,#24936,#24937,#24938,#24939,
#24940,#24941,#24942,#24943,#24944,#24945,#24946,#24947,#24948,#24949,#24950,
#24951,#24952),.UNSPECIFIED.,.F.,.F.,(4,2,2,2,2,2,2,2,4),(0.188850158043311,
0.23606157008791,0.283272982132509,0.330486649109565,0.377700316086621,
0.424913983063677,0.472127650040733,0.519339062085332,0.566550474129932),
 .UNSPECIFIED.);
#601=B_SPLINE_CURVE_WITH_KNOTS('',3,(#24954,#24955,#24956,#24957,#24958,
#24959,#24960,#24961,#24962,#24963),.UNSPECIFIED.,.F.,.F.,(4,2,2,2,4),(0.566550474129932,
0.613761886174531,0.66097329821913,0.708186965196186,0.755400632173242),
 .UNSPECIFIED.);
#602=B_SPLINE_CURVE_WITH_KNOTS('',3,(#24964,#24965,#24966,#24967,#24968,
#24969,#24970,#24971,#24972,#24973),.UNSPECIFIED.,.F.,.F.,(4,2,2,2,4),(0.755400632173242,
0.802614299150298,0.849827966127354,0.897039378171953,0.944250790216552),
 .UNSPECIFIED.);
#603=B_SPLINE_CURVE_WITH_KNOTS('',3,(#24978,#24979,#24980,#24981,#24982,
#24983,#24984,#24985,#24986,#24987,#24988,#24989,#24990,#24991,#24992,#24993,
#24994,#24995),.UNSPECIFIED.,.F.,.F.,(4,2,2,2,2,2,2,2,4),(0.,0.0474393018876097,
0.0948786037752193,0.142301138525022,0.189723673274825,0.237146208024627,
0.28456874277443,0.33200804466204,0.37944734654965),.UNSPECIFIED.);
#604=B_SPLINE_CURVE_WITH_KNOTS('',3,(#24996,#24997,#24998,#24999,#25000,
#25001,#25002,#25003,#25004,#25005,#25006,#25007,#25008,#25009,#25010,#25011,
#25012,#25013),.UNSPECIFIED.,.F.,.F.,(4,2,2,2,2,2,2,2,4),(0.37944734654965,
0.426886648437259,0.474325950324869,0.521748485074672,0.569171019824474,
0.616593554574277,0.66401608932408,0.711455391211689,0.758894693099299),
 .UNSPECIFIED.);
#605=B_SPLINE_CURVE_WITH_KNOTS('',3,(#25017,#25018,#25019,#25020,#25021,
#25022,#25023,#25024,#25025,#25026,#25027,#25028,#25029,#25030,#25031,#25032,
#25033,#25034),.UNSPECIFIED.,.F.,.F.,(4,2,2,2,2,2,2,2,4),(0.,0.0474393018876097,
0.0948786037752194,0.142301138525022,0.189723673274825,0.237146208024627,
0.28456874277443,0.33200804466204,0.37944734654965),.UNSPECIFIED.);
#606=B_SPLINE_CURVE_WITH_KNOTS('',3,(#25035,#25036,#25037,#25038,#25039,
#25040,#25041,#25042,#25043,#25044,#25045,#25046,#25047,#25048,#25049,#25050,
#25051,#25052),.UNSPECIFIED.,.F.,.F.,(4,2,2,2,2,2,2,2,4),(0.37944734654965,
0.426886648437259,0.474325950324869,0.521748485074672,0.569171019824474,
0.616593554574277,0.66401608932408,0.711455391211689,0.758894693099299),
 .UNSPECIFIED.);
#607=B_SPLINE_CURVE_WITH_KNOTS('',3,(#25420,#25421,#25422,#25423,#25424,
#25425,#25426,#25427,#25428,#25429,#25430,#25431,#25432,#25433),
 .UNSPECIFIED.,.F.,.F.,(4,2,2,2,2,2,4),(0.756005737987021,0.793568827564646,
0.872922520054201,0.952276212543756,1.03162990503331,1.11098359752286,1.14854668710049),
 .UNSPECIFIED.);
#608=B_SPLINE_CURVE_WITH_KNOTS('',3,(#25439,#25440,#25441,#25442,#25443,
#25444,#25445,#25446,#25447,#25448,#25449,#25450,#25451,#25452,#25453,#25454,
#25455,#25456),.UNSPECIFIED.,.F.,.F.,(4,2,2,2,2,2,2,2,4),(0.,0.0792165807733631,
0.158433161546726,0.23764869707457,0.316864232602414,0.396079768130258,
0.475295303658102,0.554511884431466,0.633728465204829),.UNSPECIFIED.);
#609=B_SPLINE_CURVE_WITH_KNOTS('',3,(#25457,#25458,#25459,#25460,#25461,
#25462,#25463,#25464,#25465,#25466,#25467,#25468,#25469,#25470,#25471,#25472,
#25473,#25474),.UNSPECIFIED.,.F.,.F.,(4,2,2,2,2,2,2,2,4),(0.633728465204829,
0.712945045978192,0.792161626751554,0.871377162279399,0.950592697807243,
1.02980823333509,1.10902376886293,1.18824034963629,1.26745693040966),
 .UNSPECIFIED.);
#610=B_SPLINE_CURVE_WITH_KNOTS('',3,(#25477,#25478,#25479,#25480,#25481,
#25482,#25483,#25484,#25485,#25486,#25487,#25488,#25489,#25490),
 .UNSPECIFIED.,.F.,.F.,(4,2,2,2,2,2,4),(0.121154929624517,0.158718019202143,
0.238071711691697,0.317425404181252,0.396779096670806,0.476132789160361,
0.513695878737986),.UNSPECIFIED.);
#611=B_SPLINE_CURVE_WITH_KNOTS('',3,(#25515,#25516,#25517,#25518,#25519,
#25520,#25521,#25522,#25523,#25524,#25525,#25526,#25527,#25528),
 .UNSPECIFIED.,.F.,.F.,(4,2,2,2,2,2,4),(0.756005737987017,0.793568827564644,
0.872922520054199,0.952276212543754,1.03162990503331,1.11098359752286,1.14854668710049),
 .UNSPECIFIED.);
#612=B_SPLINE_CURVE_WITH_KNOTS('',3,(#25534,#25535,#25536,#25537,#25538,
#25539,#25540,#25541,#25542,#25543,#25544,#25545,#25546,#25547,#25548,#25549,
#25550,#25551),.UNSPECIFIED.,.F.,.F.,(4,2,2,2,2,2,2,2,4),(0.,0.0792165807733624,
0.158433161546725,0.237648697074569,0.316864232602414,0.396079768130259,
0.475295303658103,0.554511884431465,0.633728465204828),.UNSPECIFIED.);
#613=B_SPLINE_CURVE_WITH_KNOTS('',3,(#25552,#25553,#25554,#25555,#25556,
#25557,#25558,#25559,#25560,#25561,#25562,#25563,#25564,#25565,#25566,#25567,
#25568,#25569),.UNSPECIFIED.,.F.,.F.,(4,2,2,2,2,2,2,2,4),(0.633728465204828,
0.71294504597819,0.792161626751553,0.871377162279397,0.950592697807242,
1.02980823333509,1.10902376886293,1.18824034963629,1.26745693040966),
 .UNSPECIFIED.);
#614=B_SPLINE_CURVE_WITH_KNOTS('',3,(#25572,#25573,#25574,#25575,#25576,
#25577,#25578,#25579,#25580,#25581,#25582,#25583,#25584,#25585),
 .UNSPECIFIED.,.F.,.F.,(4,2,2,2,2,2,4),(0.121154929624508,0.158718019202141,
0.238071711691696,0.317425404181251,0.396779096670806,0.476132789160361,
0.513695878737978),.UNSPECIFIED.);
#615=B_SPLINE_CURVE_WITH_KNOTS('',3,(#25655,#25656,#25657,#25658,#25659,
#25660,#25661,#25662,#25663,#25664,#25665,#25666,#25667,#25668),
 .UNSPECIFIED.,.F.,.F.,(4,2,2,2,2,2,4),(0.756005737987022,0.793568827564647,
0.872922520054202,0.952276212543756,1.03162990503331,1.11098359752287,1.14854668710049),
 .UNSPECIFIED.);
#616=B_SPLINE_CURVE_WITH_KNOTS('',3,(#25674,#25675,#25676,#25677,#25678,
#25679,#25680,#25681,#25682,#25683,#25684,#25685,#25686,#25687,#25688,#25689,
#25690,#25691),.UNSPECIFIED.,.F.,.F.,(4,2,2,2,2,2,2,2,4),(0.,0.079181905547237,
0.158363811094474,0.237545215630596,0.316726620166717,0.395908024702839,
0.47508942923896,0.554271334786198,0.633453240333435),.UNSPECIFIED.);
#617=B_SPLINE_CURVE_WITH_KNOTS('',3,(#25692,#25693,#25694,#25695,#25696,
#25697,#25698,#25699,#25700,#25701,#25702,#25703,#25704,#25705,#25706,#25707,
#25708,#25709),.UNSPECIFIED.,.F.,.F.,(4,2,2,2,2,2,2,2,4),(0.633453240333435,
0.712635145880671,0.791817051427908,0.87099845596403,0.950179860500152,
1.02936126503627,1.1085426695724,1.18772457511963,1.26690648066687),
 .UNSPECIFIED.);
#618=B_SPLINE_CURVE_WITH_KNOTS('',3,(#25712,#25713,#25714,#25715,#25716,
#25717,#25718,#25719,#25720,#25721,#25722,#25723,#25724,#25725),
 .UNSPECIFIED.,.F.,.F.,(4,2,2,2,2,2,4),(0.121154929624519,0.158718019202143,
0.238071711691698,0.317425404181252,0.396779096670806,0.476132789160361,
0.513695878737986),.UNSPECIFIED.);
#619=B_SPLINE_CURVE_WITH_KNOTS('',3,(#25750,#25751,#25752,#25753,#25754,
#25755,#25756,#25757,#25758,#25759,#25760,#25761,#25762,#25763),
 .UNSPECIFIED.,.F.,.F.,(4,2,2,2,2,2,4),(0.756005737987017,0.793568827564644,
0.872922520054199,0.952276212543754,1.03162990503331,1.11098359752286,1.1485466871005),
 .UNSPECIFIED.);
#620=B_SPLINE_CURVE_WITH_KNOTS('',3,(#25769,#25770,#25771,#25772,#25773,
#25774,#25775,#25776,#25777,#25778,#25779,#25780,#25781,#25782,#25783,#25784,
#25785,#25786),.UNSPECIFIED.,.F.,.F.,(4,2,2,2,2,2,2,2,4),(0.,0.0791819055472362,
0.158363811094472,0.237545215630595,0.316726620166717,0.395908024702839,
0.475089429238961,0.554271334786197,0.633453240333433),.UNSPECIFIED.);
#621=B_SPLINE_CURVE_WITH_KNOTS('',3,(#25787,#25788,#25789,#25790,#25791,
#25792,#25793,#25794,#25795,#25796,#25797,#25798,#25799,#25800,#25801,#25802,
#25803,#25804),.UNSPECIFIED.,.F.,.F.,(4,2,2,2,2,2,2,2,4),(0.633453240333433,
0.71263514588067,0.791817051427906,0.870998455964028,0.95017986050015,1.02936126503627,
1.10854266957239,1.18772457511963,1.26690648066687),.UNSPECIFIED.);
#622=B_SPLINE_CURVE_WITH_KNOTS('',3,(#25807,#25808,#25809,#25810,#25811,
#25812,#25813,#25814,#25815,#25816,#25817,#25818,#25819,#25820),
 .UNSPECIFIED.,.F.,.F.,(4,2,2,2,2,2,4),(0.121154929624508,0.158718019202141,
0.238071711691696,0.317425404181251,0.396779096670806,0.476132789160361,
0.513695878737978),.UNSPECIFIED.);
#623=B_SPLINE_CURVE_WITH_KNOTS('',3,(#25841,#25842,#25843,#25844,#25845,
#25846,#25847,#25848,#25849,#25850),.UNSPECIFIED.,.F.,.F.,(4,2,2,2,4),(0.565665723963061,
0.61280433739166,0.659942950820258,0.70708195805217,0.754220965284082),
 .UNSPECIFIED.);
#624=B_SPLINE_CURVE_WITH_KNOTS('',3,(#25852,#25853,#25854,#25855,#25856,
#25857,#25858,#25859,#25860,#25861,#25862,#25863,#25864,#25865,#25866,#25867,
#25868,#25869),.UNSPECIFIED.,.F.,.F.,(4,2,2,2,2,2,2,2,4),(0.18855524132102,
0.235693854749619,0.282832468178217,0.329971475410129,0.377110482642041,
0.424249489873953,0.471388497105864,0.518527110534463,0.565665723963061),
 .UNSPECIFIED.);
#625=B_SPLINE_CURVE_WITH_KNOTS('',3,(#25870,#25871,#25872,#25873,#25874,
#25875,#25876,#25877,#25878,#25879),.UNSPECIFIED.,.F.,.F.,(4,2,2,2,4),(0.754220965284082,
0.801359972515993,0.848498979747905,0.895637593176504,0.942776206605102),
 .UNSPECIFIED.);
#626=B_SPLINE_CURVE_WITH_KNOTS('',3,(#25883,#25884,#25885,#25886,#25887,
#25888,#25889,#25890,#25891,#25892),.UNSPECIFIED.,.F.,.F.,(4,2,2,2,4),(0.188940047579712,
0.236173496177583,0.283406944775455,0.330643519967439,0.377880095159423),
 .UNSPECIFIED.);
#627=B_SPLINE_CURVE_WITH_KNOTS('',3,(#25894,#25895,#25896,#25897,#25898,
#25899,#25900,#25901,#25902,#25903),.UNSPECIFIED.,.F.,.F.,(4,2,2,2,4),(0.,
0.0472365751919841,0.0944731503839682,0.14170659898184,0.188940047579712),
 .UNSPECIFIED.);
#628=B_SPLINE_CURVE_WITH_KNOTS('',3,(#25905,#25906,#25907,#25908,#25909,
#25910,#25911,#25912,#25913,#25914),.UNSPECIFIED.,.F.,.F.,(4,2,2,2,4),(0.566820142739135,
0.614053591337007,0.661287039934879,0.708523615126863,0.755760190318847),
 .UNSPECIFIED.);
#629=B_SPLINE_CURVE_WITH_KNOTS('',3,(#25915,#25916,#25917,#25918,#25919,
#25920,#25921,#25922,#25923,#25924),.UNSPECIFIED.,.F.,.F.,(4,2,2,2,4),(0.377880095159423,
0.425116670351408,0.472353245543392,0.519586694141263,0.566820142739135),
 .UNSPECIFIED.);
#630=B_SPLINE_CURVE_WITH_KNOTS('',3,(#25928,#25929,#25930,#25931,#25932,
#25933,#25934,#25935,#25936,#25937,#25938,#25939,#25940,#25941,#25942,#25943,
#25944,#25945),.UNSPECIFIED.,.F.,.F.,(4,2,2,2,2,2,2,2,4),(0.,0.0472365751919841,
0.0944731503839683,0.14170659898184,0.188940047579712,0.236173496177583,
0.283406944775455,0.330643519967439,0.377880095159423),.UNSPECIFIED.);
#631=B_SPLINE_CURVE_WITH_KNOTS('',3,(#25946,#25947,#25948,#25949,#25950,
#25951,#25952,#25953,#25954,#25955,#25956,#25957,#25958,#25959,#25960,#25961,
#25962,#25963),.UNSPECIFIED.,.F.,.F.,(4,2,2,2,2,2,2,2,4),(0.377880095159423,
0.425116670351408,0.472353245543392,0.519586694141263,0.566820142739135,
0.614053591337007,0.661287039934879,0.708523615126863,0.755760190318847),
 .UNSPECIFIED.);
#632=B_SPLINE_CURVE_WITH_KNOTS('',3,(#25967,#25968,#25969,#25970,#25971,
#25972,#25973,#25974,#25975,#25976),.UNSPECIFIED.,.F.,.F.,(4,2,2,2,4),(0.565665723963061,
0.61280433739166,0.659942950820258,0.70708195805217,0.754220965284082),
 .UNSPECIFIED.);
#633=B_SPLINE_CURVE_WITH_KNOTS('',3,(#25978,#25979,#25980,#25981,#25982,
#25983,#25984,#25985,#25986,#25987,#25988,#25989,#25990,#25991,#25992,#25993,
#25994,#25995),.UNSPECIFIED.,.F.,.F.,(4,2,2,2,2,2,2,2,4),(0.18855524132102,
0.235693854749619,0.282832468178217,0.329971475410129,0.377110482642041,
0.424249489873953,0.471388497105864,0.518527110534463,0.565665723963061),
 .UNSPECIFIED.);
#634=B_SPLINE_CURVE_WITH_KNOTS('',3,(#25996,#25997,#25998,#25999,#26000,
#26001,#26002,#26003,#26004,#26005),.UNSPECIFIED.,.F.,.F.,(4,2,2,2,4),(0.754220965284082,
0.801359972515993,0.848498979747905,0.895637593176504,0.942776206605102),
 .UNSPECIFIED.);
#635=B_SPLINE_CURVE_WITH_KNOTS('',3,(#26015,#26016,#26017,#26018,#26019,
#26020,#26021,#26022,#26023,#26024,#26025,#26026,#26027,#26028,#26029,#26030,
#26031,#26032),.UNSPECIFIED.,.F.,.F.,(4,2,2,2,2,2,2,2,4),(0.18855524132102,
0.235693854749619,0.282832468178217,0.329971475410129,0.377110482642041,
0.424249489873953,0.471388497105864,0.518527110534463,0.565665723963061),
 .UNSPECIFIED.);
#636=B_SPLINE_CURVE_WITH_KNOTS('',3,(#26034,#26035,#26036,#26037,#26038,
#26039,#26040,#26041,#26042,#26043),.UNSPECIFIED.,.F.,.F.,(4,2,2,2,4),(0.565665723963061,
0.61280433739166,0.659942950820258,0.70708195805217,0.754220965284082),
 .UNSPECIFIED.);
#637=B_SPLINE_CURVE_WITH_KNOTS('',3,(#26044,#26045,#26046,#26047,#26048,
#26049,#26050,#26051,#26052,#26053),.UNSPECIFIED.,.F.,.F.,(4,2,2,2,4),(0.754220965284082,
0.801359972515993,0.848498979747905,0.895637593176504,0.942776206605102),
 .UNSPECIFIED.);
#638=B_SPLINE_CURVE_WITH_KNOTS('',3,(#26056,#26057,#26058,#26059,#26060,
#26061,#26062,#26063,#26064,#26065,#26066,#26067,#26068,#26069,#26070,#26071,
#26072,#26073),.UNSPECIFIED.,.F.,.F.,(4,2,2,2,2,2,2,2,4),(0.18855524132102,
0.235693854749619,0.282832468178217,0.329971475410129,0.377110482642041,
0.424249489873953,0.471388497105864,0.518527110534463,0.565665723963061),
 .UNSPECIFIED.);
#639=B_SPLINE_CURVE_WITH_KNOTS('',3,(#26075,#26076,#26077,#26078,#26079,
#26080,#26081,#26082,#26083,#26084),.UNSPECIFIED.,.F.,.F.,(4,2,2,2,4),(0.565665723963061,
0.61280433739166,0.659942950820258,0.70708195805217,0.754220965284082),
 .UNSPECIFIED.);
#640=B_SPLINE_CURVE_WITH_KNOTS('',3,(#26085,#26086,#26087,#26088,#26089,
#26090,#26091,#26092,#26093,#26094),.UNSPECIFIED.,.F.,.F.,(4,2,2,2,4),(0.754220965284082,
0.801359972515993,0.848498979747905,0.895637593176504,0.942776206605102),
 .UNSPECIFIED.);
#641=B_SPLINE_CURVE_WITH_KNOTS('',3,(#26099,#26100,#26101,#26102,#26103,
#26104,#26105,#26106,#26107,#26108,#26109,#26110,#26111,#26112,#26113,#26114,
#26115,#26116),.UNSPECIFIED.,.F.,.F.,(4,2,2,2,2,2,2,2,4),(0.,0.0472365751919841,
0.0944731503839683,0.14170659898184,0.188940047579712,0.236173496177583,
0.283406944775455,0.330643519967439,0.377880095159424),.UNSPECIFIED.);
#642=B_SPLINE_CURVE_WITH_KNOTS('',3,(#26117,#26118,#26119,#26120,#26121,
#26122,#26123,#26124,#26125,#26126,#26127,#26128,#26129,#26130,#26131,#26132,
#26133,#26134),.UNSPECIFIED.,.F.,.F.,(4,2,2,2,2,2,2,2,4),(0.377880095159424,
0.425116670351408,0.472353245543392,0.519586694141263,0.566820142739135,
0.614053591337007,0.661287039934879,0.708523615126863,0.755760190318847),
 .UNSPECIFIED.);
#643=B_SPLINE_CURVE_WITH_KNOTS('',3,(#26138,#26139,#26140,#26141,#26142,
#26143,#26144,#26145,#26146,#26147,#26148,#26149,#26150,#26151,#26152,#26153,
#26154,#26155),.UNSPECIFIED.,.F.,.F.,(4,2,2,2,2,2,2,2,4),(0.,0.0472365751919841,
0.0944731503839683,0.14170659898184,0.188940047579712,0.236173496177583,
0.283406944775455,0.330643519967439,0.377880095159423),.UNSPECIFIED.);
#644=B_SPLINE_CURVE_WITH_KNOTS('',3,(#26156,#26157,#26158,#26159,#26160,
#26161,#26162,#26163,#26164,#26165,#26166,#26167,#26168,#26169,#26170,#26171,
#26172,#26173),.UNSPECIFIED.,.F.,.F.,(4,2,2,2,2,2,2,2,4),(0.377880095159423,
0.425116670351408,0.472353245543392,0.519586694141263,0.566820142739135,
0.614053591337007,0.661287039934879,0.708523615126863,0.755760190318847),
 .UNSPECIFIED.);
#645=SPHERICAL_SURFACE('',#15231,0.23815);
#646=SPHERICAL_SURFACE('',#15233,0.23815);
#647=SPHERICAL_SURFACE('',#15235,0.23815);
#648=SPHERICAL_SURFACE('',#15237,0.23815);
#649=SPHERICAL_SURFACE('',#15239,0.23815);
#650=SPHERICAL_SURFACE('',#15241,0.23815);
#651=SPHERICAL_SURFACE('',#15243,0.23815);
#652=SPHERICAL_SURFACE('',#15245,0.23815);
#653=SPHERICAL_SURFACE('',#15248,0.247676);
#654=SPHERICAL_SURFACE('',#15264,0.247676);
#655=SPHERICAL_SURFACE('',#15269,0.247676);
#656=SPHERICAL_SURFACE('',#15274,0.247676);
#657=SPHERICAL_SURFACE('',#15279,0.247676);
#658=SPHERICAL_SURFACE('',#15284,0.247676);
#659=SPHERICAL_SURFACE('',#15289,0.247676);
#660=SPHERICAL_SURFACE('',#15297,0.247676);
#661=SPHERICAL_SURFACE('',#15395,0.29765);
#662=SPHERICAL_SURFACE('',#15397,0.29765);
#663=SPHERICAL_SURFACE('',#15399,0.29765);
#664=SPHERICAL_SURFACE('',#15401,0.29765);
#665=SPHERICAL_SURFACE('',#15403,0.29765);
#666=SPHERICAL_SURFACE('',#15405,0.29765);
#667=SPHERICAL_SURFACE('',#15407,0.29765);
#668=SPHERICAL_SURFACE('',#15410,0.309556);
#669=SPHERICAL_SURFACE('',#15426,0.309556);
#670=SPHERICAL_SURFACE('',#15431,0.309556);
#671=SPHERICAL_SURFACE('',#15437,0.309556);
#672=SPHERICAL_SURFACE('',#15442,0.309556);
#673=SPHERICAL_SURFACE('',#15447,0.309556);
#674=SPHERICAL_SURFACE('',#15455,0.309556);
#675=SPHERICAL_SURFACE('',#15515,2.35);
#676=SPHERICAL_SURFACE('',#15555,2.35);
#677=CONICAL_SURFACE('',#15202,0.53,0.785398163397448);
#678=CONICAL_SURFACE('',#15209,0.53,0.785398163397448);
#679=CONICAL_SURFACE('',#15222,1.47,0.785398163397449);
#680=CONICAL_SURFACE('',#15226,1.47,0.785398163397449);
#681=CONICAL_SURFACE('',#15340,0.325,0.785398163397448);
#682=CONICAL_SURFACE('',#15344,0.335,0.785398163397448);
#683=CONICAL_SURFACE('',#15348,0.21,0.463647609000806);
#684=CONICAL_SURFACE('',#15352,0.18,0.785398163397448);
#685=CONICAL_SURFACE('',#15366,0.63,0.785398163397448);
#686=CONICAL_SURFACE('',#15373,0.63,0.785398163397448);
#687=CONICAL_SURFACE('',#15386,1.57,0.785398163397449);
#688=CONICAL_SURFACE('',#15390,1.57,0.785398163397449);
#689=CONICAL_SURFACE('',#15484,0.4,0.785398163397448);
#690=CONICAL_SURFACE('',#15488,0.41,0.785398163397448);
#691=CONICAL_SURFACE('',#15492,0.26,0.463647609000806);
#692=CONICAL_SURFACE('',#15496,0.225,0.785398163397448);
#693=CONICAL_SURFACE('',#15601,0.625,0.785398163397448);
#694=CONICAL_SURFACE('',#15605,0.635,0.785398163397449);
#695=CONICAL_SURFACE('',#15609,0.41,0.463647609000806);
#696=CONICAL_SURFACE('',#15625,0.325,0.785398163397448);
#697=CONICAL_SURFACE('',#15629,0.335,0.785398163397448);
#698=CONICAL_SURFACE('',#15633,0.21,0.463647609000806);
#699=CONICAL_SURFACE('',#16281,0.325,0.785398163397448);
#700=CONICAL_SURFACE('',#16285,0.335,0.785398163397448);
#701=CONICAL_SURFACE('',#16289,0.21,0.463647609000806);
#702=CONICAL_SURFACE('',#16293,0.18,0.785398163397448);
#703=CONICAL_SURFACE('',#16393,0.235,0.785398163397448);
#704=CONICAL_SURFACE('',#16397,0.2125,0.785398163397448);
#705=TOROIDAL_SURFACE('',#15191,1.,0.247676);
#706=TOROIDAL_SURFACE('',#15211,1.,0.247676);
#707=TOROIDAL_SURFACE('',#15355,1.1,0.309556);
#708=TOROIDAL_SURFACE('',#15375,1.1,0.309556);
#709=SHAPE_REPRESENTATION_RELATIONSHIP('SRR','None',#27353,#778);
#710=SHAPE_REPRESENTATION_RELATIONSHIP('SRR','None',#27354,#779);
#711=SHAPE_REPRESENTATION_RELATIONSHIP('SRR','None',#27355,#780);
#712=SHAPE_REPRESENTATION_RELATIONSHIP('SRR','None',#27356,#781);
#713=SHAPE_REPRESENTATION_RELATIONSHIP('SRR','None',#27357,#782);
#714=SHAPE_REPRESENTATION_RELATIONSHIP('SRR','None',#27358,#783);
#715=SHAPE_REPRESENTATION_RELATIONSHIP('SRR','None',#27359,#784);
#716=SHAPE_REPRESENTATION_RELATIONSHIP('SRR','None',#27360,#785);
#717=SHAPE_REPRESENTATION_RELATIONSHIP('SRR','None',#27361,#786);
#718=SHAPE_REPRESENTATION_RELATIONSHIP('SRR','None',#27362,#787);
#719=SHAPE_REPRESENTATION_RELATIONSHIP('SRR','None',#27363,#788);
#720=SHAPE_REPRESENTATION_RELATIONSHIP('SRR','None',#27364,#789);
#721=SHAPE_REPRESENTATION_RELATIONSHIP('SRR','None',#27365,#790);
#722=SHAPE_REPRESENTATION_RELATIONSHIP('SRR','None',#27366,#791);
#723=SHAPE_REPRESENTATION_RELATIONSHIP('SRR','None',#27367,#792);
#724=SHAPE_REPRESENTATION_RELATIONSHIP('SRR','None',#27368,#793);
#725=SHAPE_REPRESENTATION_RELATIONSHIP('SRR','None',#27369,#794);
#726=SHAPE_REPRESENTATION_RELATIONSHIP('SRR','None',#27370,#795);
#727=SHAPE_REPRESENTATION_RELATIONSHIP('SRR','None',#27371,#796);
#728=SHAPE_REPRESENTATION_RELATIONSHIP('SRR','None',#27372,#797);
#729=SHAPE_REPRESENTATION_RELATIONSHIP('SRR','None',#27373,#798);
#730=SHAPE_REPRESENTATION_RELATIONSHIP('SRR','None',#27374,#799);
#731=SHAPE_REPRESENTATION_RELATIONSHIP('SRR','None',#27375,#800);
#732=SHAPE_REPRESENTATION_RELATIONSHIP('SRR','None',#27376,#801);
#733=SHAPE_REPRESENTATION_RELATIONSHIP('SRR','None',#27377,#802);
#734=SHAPE_REPRESENTATION_RELATIONSHIP('SRR','None',#27378,#803);
#735=SHAPE_REPRESENTATION_RELATIONSHIP('SRR','None',#27379,#804);
#736=SHAPE_REPRESENTATION_RELATIONSHIP('SRR','None',#27381,#805);
#737=SHAPE_REPRESENTATION_RELATIONSHIP('SRR','None',#27382,#806);
#738=SHAPE_REPRESENTATION_RELATIONSHIP('SRR','None',#27383,#807);
#739=SHAPE_REPRESENTATION_RELATIONSHIP('SRR','None',#27384,#808);
#740=SHAPE_REPRESENTATION_RELATIONSHIP('SRR','None',#27385,#809);
#741=SHAPE_REPRESENTATION_RELATIONSHIP('SRR','None',#27386,#810);
#742=SHAPE_REPRESENTATION_RELATIONSHIP('SRR','None',#27388,#811);
#743=SHAPE_REPRESENTATION_RELATIONSHIP('SRR','None',#27389,#812);
#744=SHAPE_REPRESENTATION_RELATIONSHIP('SRR','None',#27390,#813);
#745=SHAPE_REPRESENTATION_RELATIONSHIP('SRR','None',#27391,#814);
#746=SHAPE_REPRESENTATION_RELATIONSHIP('SRR','None',#27392,#815);
#747=SHAPE_REPRESENTATION_RELATIONSHIP('SRR','None',#27393,#816);
#748=SHAPE_REPRESENTATION_RELATIONSHIP('SRR','None',#27395,#817);
#749=SHAPE_REPRESENTATION_RELATIONSHIP('SRR','None',#27396,#818);
#750=SHAPE_REPRESENTATION_RELATIONSHIP('SRR','None',#27397,#819);
#751=SHAPE_REPRESENTATION_RELATIONSHIP('SRR','None',#27398,#820);
#752=SHAPE_REPRESENTATION_RELATIONSHIP('SRR','None',#27399,#821);
#753=SHAPE_REPRESENTATION_RELATIONSHIP('SRR','None',#27401,#822);
#754=SHAPE_REPRESENTATION_RELATIONSHIP('SRR','None',#27402,#823);
#755=SHAPE_REPRESENTATION_RELATIONSHIP('SRR','None',#27403,#824);
#756=SHAPE_REPRESENTATION_RELATIONSHIP('SRR','None',#27404,#825);
#757=SHAPE_REPRESENTATION_RELATIONSHIP('SRR','None',#27405,#826);
#758=SHAPE_REPRESENTATION_RELATIONSHIP('SRR','None',#27406,#827);
#759=SHAPE_REPRESENTATION_RELATIONSHIP('SRR','None',#27407,#828);
#760=SHAPE_REPRESENTATION_RELATIONSHIP('SRR','None',#27408,#829);
#761=SHAPE_REPRESENTATION_RELATIONSHIP('SRR','None',#27409,#830);
#762=SHAPE_REPRESENTATION_RELATIONSHIP('SRR','None',#27411,#831);
#763=SHAPE_REPRESENTATION_RELATIONSHIP('SRR','None',#27412,#832);
#764=SHAPE_REPRESENTATION_RELATIONSHIP('SRR','None',#27413,#833);
#765=SHAPE_REPRESENTATION_RELATIONSHIP('SRR','None',#27414,#834);
#766=SHAPE_REPRESENTATION_RELATIONSHIP('SRR','None',#27415,#835);
#767=SHAPE_REPRESENTATION_RELATIONSHIP('SRR','None',#27416,#836);
#768=SHAPE_REPRESENTATION_RELATIONSHIP('SRR','None',#27417,#837);
#769=SHAPE_REPRESENTATION_RELATIONSHIP('SRR','None',#27418,#838);
#770=SHAPE_REPRESENTATION_RELATIONSHIP('SRR','None',#27419,#839);
#771=SHAPE_REPRESENTATION_RELATIONSHIP('SRR','None',#27420,#840);
#772=SHAPE_REPRESENTATION_RELATIONSHIP('SRR','None',#27421,#841);
#773=SHAPE_REPRESENTATION_RELATIONSHIP('SRR','None',#27422,#842);
#774=SHAPE_REPRESENTATION_RELATIONSHIP('SRR','None',#27423,#843);
#775=SHAPE_REPRESENTATION_RELATIONSHIP('SRR','None',#27424,#844);
#776=SHAPE_REPRESENTATION_RELATIONSHIP('SRR','None',#27425,#845);
#777=SHAPE_REPRESENTATION_RELATIONSHIP('SRR','None',#27426,#846);
#778=ADVANCED_BREP_SHAPE_REPRESENTATION('',(#932),#26995);
#779=ADVANCED_BREP_SHAPE_REPRESENTATION('',(#933),#26996);
#780=ADVANCED_BREP_SHAPE_REPRESENTATION('',(#934),#26997);
#781=ADVANCED_BREP_SHAPE_REPRESENTATION('',(#935),#26998);
#782=ADVANCED_BREP_SHAPE_REPRESENTATION('',(#936),#26999);
#783=ADVANCED_BREP_SHAPE_REPRESENTATION('',(#937),#27000);
#784=ADVANCED_BREP_SHAPE_REPRESENTATION('',(#938),#27001);
#785=ADVANCED_BREP_SHAPE_REPRESENTATION('',(#939),#27002);
#786=ADVANCED_BREP_SHAPE_REPRESENTATION('',(#940),#27003);
#787=ADVANCED_BREP_SHAPE_REPRESENTATION('',(#941),#27004);
#788=ADVANCED_BREP_SHAPE_REPRESENTATION('',(#942),#27005);
#789=ADVANCED_BREP_SHAPE_REPRESENTATION('',(#943),#27006);
#790=ADVANCED_BREP_SHAPE_REPRESENTATION('',(#944),#27007);
#791=ADVANCED_BREP_SHAPE_REPRESENTATION('',(#945),#27008);
#792=ADVANCED_BREP_SHAPE_REPRESENTATION('',(#946),#27009);
#793=ADVANCED_BREP_SHAPE_REPRESENTATION('',(#947),#27010);
#794=ADVANCED_BREP_SHAPE_REPRESENTATION('',(#948),#27011);
#795=ADVANCED_BREP_SHAPE_REPRESENTATION('',(#949),#27012);
#796=ADVANCED_BREP_SHAPE_REPRESENTATION('',(#950),#27013);
#797=ADVANCED_BREP_SHAPE_REPRESENTATION('',(#951),#27014);
#798=ADVANCED_BREP_SHAPE_REPRESENTATION('',(#952),#27015);
#799=ADVANCED_BREP_SHAPE_REPRESENTATION('',(#953),#27016);
#800=ADVANCED_BREP_SHAPE_REPRESENTATION('',(#954),#27017);
#801=ADVANCED_BREP_SHAPE_REPRESENTATION('',(#955),#27018);
#802=ADVANCED_BREP_SHAPE_REPRESENTATION('',(#956),#27019);
#803=ADVANCED_BREP_SHAPE_REPRESENTATION('',(#957),#27020);
#804=ADVANCED_BREP_SHAPE_REPRESENTATION('',(#958),#27021);
#805=ADVANCED_BREP_SHAPE_REPRESENTATION('',(#959),#27023);
#806=ADVANCED_BREP_SHAPE_REPRESENTATION('',(#960),#27024);
#807=ADVANCED_BREP_SHAPE_REPRESENTATION('',(#961,#962,#963,#964,#965,#966,
#967,#968),#27025);
#808=ADVANCED_BREP_SHAPE_REPRESENTATION('',(#969),#27026);
#809=ADVANCED_BREP_SHAPE_REPRESENTATION('',(#970,#971),#27027);
#810=ADVANCED_BREP_SHAPE_REPRESENTATION('',(#16),#27028);
#811=ADVANCED_BREP_SHAPE_REPRESENTATION('',(#972),#27030);
#812=ADVANCED_BREP_SHAPE_REPRESENTATION('',(#973),#27031);
#813=ADVANCED_BREP_SHAPE_REPRESENTATION('',(#974,#975,#976,#977,#978,#979,
#980),#27032);
#814=ADVANCED_BREP_SHAPE_REPRESENTATION('',(#981),#27033);
#815=ADVANCED_BREP_SHAPE_REPRESENTATION('',(#982,#983),#27034);
#816=ADVANCED_BREP_SHAPE_REPRESENTATION('',(#17),#27035);
#817=ADVANCED_BREP_SHAPE_REPRESENTATION('',(#984),#27037);
#818=ADVANCED_BREP_SHAPE_REPRESENTATION('',(#985,#986),#27038);
#819=ADVANCED_BREP_SHAPE_REPRESENTATION('',(#987),#27039);
#820=ADVANCED_BREP_SHAPE_REPRESENTATION('',(#18),#27040);
#821=ADVANCED_BREP_SHAPE_REPRESENTATION('',(#19),#27041);
#822=ADVANCED_BREP_SHAPE_REPRESENTATION('',(#988),#27043);
#823=ADVANCED_BREP_SHAPE_REPRESENTATION('',(#989),#27044);
#824=ADVANCED_BREP_SHAPE_REPRESENTATION('',(#990),#27045);
#825=ADVANCED_BREP_SHAPE_REPRESENTATION('',(#991),#27046);
#826=ADVANCED_BREP_SHAPE_REPRESENTATION('',(#992),#27047);
#827=ADVANCED_BREP_SHAPE_REPRESENTATION('',(#993),#27048);
#828=ADVANCED_BREP_SHAPE_REPRESENTATION('',(#994),#27049);
#829=ADVANCED_BREP_SHAPE_REPRESENTATION('',(#995),#27050);
#830=ADVANCED_BREP_SHAPE_REPRESENTATION('',(#996),#27051);
#831=ADVANCED_BREP_SHAPE_REPRESENTATION('',(#997),#27053);
#832=ADVANCED_BREP_SHAPE_REPRESENTATION('',(#998),#27054);
#833=ADVANCED_BREP_SHAPE_REPRESENTATION('',(#999),#27055);
#834=ADVANCED_BREP_SHAPE_REPRESENTATION('',(#1000),#27056);
#835=ADVANCED_BREP_SHAPE_REPRESENTATION('',(#1001),#27057);
#836=ADVANCED_BREP_SHAPE_REPRESENTATION('',(#1002),#27058);
#837=ADVANCED_BREP_SHAPE_REPRESENTATION('',(#1003),#27059);
#838=ADVANCED_BREP_SHAPE_REPRESENTATION('',(#1004),#27060);
#839=ADVANCED_BREP_SHAPE_REPRESENTATION('',(#1005),#27061);
#840=ADVANCED_BREP_SHAPE_REPRESENTATION('',(#1006),#27062);
#841=ADVANCED_BREP_SHAPE_REPRESENTATION('',(#1007),#27063);
#842=ADVANCED_BREP_SHAPE_REPRESENTATION('',(#1008),#27064);
#843=ADVANCED_BREP_SHAPE_REPRESENTATION('',(#1009),#27065);
#844=ADVANCED_BREP_SHAPE_REPRESENTATION('',(#1010),#27066);
#845=ADVANCED_BREP_SHAPE_REPRESENTATION('',(#20),#27067);
#846=ADVANCED_BREP_SHAPE_REPRESENTATION('',(#1011),#27068);
#847=STYLED_ITEM('',(#27776),#932);
#848=STYLED_ITEM('',(#27811),#933);
#849=STYLED_ITEM('',(#27811),#934);
#850=STYLED_ITEM('',(#27797),#935);
#851=STYLED_ITEM('',(#27790),#936);
#852=STYLED_ITEM('',(#27797),#937);
#853=STYLED_ITEM('',(#27797),#938);
#854=STYLED_ITEM('',(#27797),#939);
#855=STYLED_ITEM('',(#27804),#940);
#856=STYLED_ITEM('',(#27804),#941);
#857=STYLED_ITEM('',(#27804),#942);
#858=STYLED_ITEM('',(#27804),#943);
#859=STYLED_ITEM('',(#27811),#944);
#860=STYLED_ITEM('',(#27797),#945);
#861=STYLED_ITEM('',(#27797),#946);
#862=STYLED_ITEM('',(#27804),#947);
#863=STYLED_ITEM('',(#27797),#948);
#864=STYLED_ITEM('',(#27797),#949);
#865=STYLED_ITEM('',(#27797),#950);
#866=STYLED_ITEM('',(#27797),#951);
#867=STYLED_ITEM('',(#27797),#952);
#868=STYLED_ITEM('',(#27797),#953);
#869=STYLED_ITEM('',(#27783),#954);
#870=STYLED_ITEM('',(#27790),#955);
#871=STYLED_ITEM('',(#27790),#956);
#872=STYLED_ITEM('',(#27790),#957);
#873=STYLED_ITEM('',(#27804),#958);
#874=STYLED_ITEM('',(#27797),#959);
#875=STYLED_ITEM('',(#27797),#960);
#876=STYLED_ITEM('',(#27797),#961);
#877=STYLED_ITEM('',(#27797),#962);
#878=STYLED_ITEM('',(#27797),#963);
#879=STYLED_ITEM('',(#27797),#964);
#880=STYLED_ITEM('',(#27797),#965);
#881=STYLED_ITEM('',(#27797),#966);
#882=STYLED_ITEM('',(#27797),#967);
#883=STYLED_ITEM('',(#27797),#968);
#884=STYLED_ITEM('',(#27797),#969);
#885=STYLED_ITEM('',(#27797),#970);
#886=STYLED_ITEM('',(#27797),#971);
#887=STYLED_ITEM('',(#27804),#16);
#888=STYLED_ITEM('',(#27797),#972);
#889=STYLED_ITEM('',(#27797),#973);
#890=STYLED_ITEM('',(#27797),#974);
#891=STYLED_ITEM('',(#27797),#975);
#892=STYLED_ITEM('',(#27797),#976);
#893=STYLED_ITEM('',(#27797),#977);
#894=STYLED_ITEM('',(#27797),#978);
#895=STYLED_ITEM('',(#27797),#979);
#896=STYLED_ITEM('',(#27797),#980);
#897=STYLED_ITEM('',(#27797),#981);
#898=STYLED_ITEM('',(#27797),#982);
#899=STYLED_ITEM('',(#27797),#983);
#900=STYLED_ITEM('',(#27804),#17);
#901=STYLED_ITEM('',(#27776),#984);
#902=STYLED_ITEM('',(#27797),#985);
#903=STYLED_ITEM('',(#27797),#986);
#904=STYLED_ITEM('',(#27804),#987);
#905=STYLED_ITEM('',(#27804),#18);
#906=STYLED_ITEM('',(#27804),#19);
#907=STYLED_ITEM('',(#27797),#988);
#908=STYLED_ITEM('',(#27811),#989);
#909=STYLED_ITEM('',(#27783),#990);
#910=STYLED_ITEM('',(#27804),#991);
#911=STYLED_ITEM('',(#27804),#992);
#912=STYLED_ITEM('',(#27790),#993);
#913=STYLED_ITEM('',(#27797),#994);
#914=STYLED_ITEM('',(#27783),#995);
#915=STYLED_ITEM('',(#27811),#996);
#916=STYLED_ITEM('',(#27797),#997);
#917=STYLED_ITEM('',(#27790),#998);
#918=STYLED_ITEM('',(#27790),#999);
#919=STYLED_ITEM('',(#27804),#1000);
#920=STYLED_ITEM('',(#27804),#1001);
#921=STYLED_ITEM('',(#27811),#1002);
#922=STYLED_ITEM('',(#27797),#1003);
#923=STYLED_ITEM('',(#27797),#1004);
#924=STYLED_ITEM('',(#27811),#1005);
#925=STYLED_ITEM('',(#27790),#1006);
#926=STYLED_ITEM('',(#27790),#1007);
#927=STYLED_ITEM('',(#27783),#1008);
#928=STYLED_ITEM('',(#27783),#1009);
#929=STYLED_ITEM('',(#27790),#1010);
#930=STYLED_ITEM('',(#27804),#20);
#931=STYLED_ITEM('',(#27804),#1011);
#932=MANIFOLD_SOLID_BREP('Body1',#13712);
#933=MANIFOLD_SOLID_BREP('Body1',#13713);
#934=MANIFOLD_SOLID_BREP('Body1',#13714);
#935=MANIFOLD_SOLID_BREP('Body1',#13715);
#936=MANIFOLD_SOLID_BREP('Body1',#13716);
#937=MANIFOLD_SOLID_BREP('Body1',#13717);
#938=MANIFOLD_SOLID_BREP('Body1',#13718);
#939=MANIFOLD_SOLID_BREP('Body1',#13719);
#940=MANIFOLD_SOLID_BREP('Body1',#13720);
#941=MANIFOLD_SOLID_BREP('Body1',#13721);
#942=MANIFOLD_SOLID_BREP('Body1',#13722);
#943=MANIFOLD_SOLID_BREP('Body1',#13723);
#944=MANIFOLD_SOLID_BREP('Body1',#13724);
#945=MANIFOLD_SOLID_BREP('Body1',#13725);
#946=MANIFOLD_SOLID_BREP('Body1',#13726);
#947=MANIFOLD_SOLID_BREP('Body1',#13727);
#948=MANIFOLD_SOLID_BREP('Body1',#13728);
#949=MANIFOLD_SOLID_BREP('Body1',#13729);
#950=MANIFOLD_SOLID_BREP('Body1',#13730);
#951=MANIFOLD_SOLID_BREP('Body1',#13731);
#952=MANIFOLD_SOLID_BREP('Body1',#13732);
#953=MANIFOLD_SOLID_BREP('Body1',#13733);
#954=MANIFOLD_SOLID_BREP('Body1',#13734);
#955=MANIFOLD_SOLID_BREP('Body1',#13735);
#956=MANIFOLD_SOLID_BREP('Body1',#13736);
#957=MANIFOLD_SOLID_BREP('Body1',#13737);
#958=MANIFOLD_SOLID_BREP('Body1',#13738);
#959=MANIFOLD_SOLID_BREP('Body1',#13739);
#960=MANIFOLD_SOLID_BREP('Body1',#13740);
#961=MANIFOLD_SOLID_BREP('Body1',#13741);
#962=MANIFOLD_SOLID_BREP('Body2',#13742);
#963=MANIFOLD_SOLID_BREP('Body3',#13743);
#964=MANIFOLD_SOLID_BREP('Body4',#13744);
#965=MANIFOLD_SOLID_BREP('Body5',#13745);
#966=MANIFOLD_SOLID_BREP('Body6',#13746);
#967=MANIFOLD_SOLID_BREP('Body7',#13747);
#968=MANIFOLD_SOLID_BREP('Body8',#13748);
#969=MANIFOLD_SOLID_BREP('Continuous crown cage',#13749);
#970=MANIFOLD_SOLID_BREP('Body1',#13750);
#971=MANIFOLD_SOLID_BREP('Body2',#13751);
#972=MANIFOLD_SOLID_BREP('Body1',#13754);
#973=MANIFOLD_SOLID_BREP('Body1',#13755);
#974=MANIFOLD_SOLID_BREP('Body1',#13756);
#975=MANIFOLD_SOLID_BREP('Body2',#13757);
#976=MANIFOLD_SOLID_BREP('Body3',#13758);
#977=MANIFOLD_SOLID_BREP('Body4',#13759);
#978=MANIFOLD_SOLID_BREP('Body5',#13760);
#979=MANIFOLD_SOLID_BREP('Body6',#13761);
#980=MANIFOLD_SOLID_BREP('Body7',#13762);
#981=MANIFOLD_SOLID_BREP('Continuous crown cage',#13763);
#982=MANIFOLD_SOLID_BREP('Body1',#13764);
#983=MANIFOLD_SOLID_BREP('Body2',#13765);
#984=MANIFOLD_SOLID_BREP('Body1',#13768);
#985=MANIFOLD_SOLID_BREP('Body1',#13769);
#986=MANIFOLD_SOLID_BREP('Body2',#13770);
#987=MANIFOLD_SOLID_BREP('Body1',#13771);
#988=MANIFOLD_SOLID_BREP('Body1',#13776);
#989=MANIFOLD_SOLID_BREP('Body1',#13777);
#990=MANIFOLD_SOLID_BREP('Body1',#13778);
#991=MANIFOLD_SOLID_BREP('Body1',#13779);
#992=MANIFOLD_SOLID_BREP('Body1',#13780);
#993=MANIFOLD_SOLID_BREP('Body1',#13781);
#994=MANIFOLD_SOLID_BREP('Body1',#13782);
#995=MANIFOLD_SOLID_BREP('Body1',#13783);
#996=MANIFOLD_SOLID_BREP('Body1',#13784);
#997=MANIFOLD_SOLID_BREP('Body1',#13785);
#998=MANIFOLD_SOLID_BREP('Body1',#13786);
#999=MANIFOLD_SOLID_BREP('Body1',#13787);
#1000=MANIFOLD_SOLID_BREP('Body1',#13788);
#1001=MANIFOLD_SOLID_BREP('Body1',#13789);
#1002=MANIFOLD_SOLID_BREP('Body1',#13790);
#1003=MANIFOLD_SOLID_BREP('Body1',#13791);
#1004=MANIFOLD_SOLID_BREP('Body1',#13792);
#1005=MANIFOLD_SOLID_BREP('Body1',#13793);
#1006=MANIFOLD_SOLID_BREP('Body1',#13794);
#1007=MANIFOLD_SOLID_BREP('Body1',#13795);
#1008=MANIFOLD_SOLID_BREP('Body1',#13796);
#1009=MANIFOLD_SOLID_BREP('Body1',#13797);
#1010=MANIFOLD_SOLID_BREP('Body1',#13798);
#1011=MANIFOLD_SOLID_BREP('Body1',#13801);
#1012=FACE_BOUND('',#2456,.T.);
#1013=FACE_BOUND('',#2457,.T.);
#1014=FACE_BOUND('',#2458,.T.);
#1015=FACE_BOUND('',#2459,.T.);
#1016=FACE_BOUND('',#2487,.T.);
#1017=FACE_BOUND('',#2488,.T.);
#1018=FACE_BOUND('',#2489,.T.);
#1019=FACE_BOUND('',#2490,.T.);
#1020=FACE_BOUND('',#2491,.T.);
#1021=FACE_BOUND('',#2492,.T.);
#1022=FACE_BOUND('',#2493,.T.);
#1023=FACE_BOUND('',#2494,.T.);
#1024=FACE_BOUND('',#2495,.T.);
#1025=FACE_BOUND('',#2496,.T.);
#1026=FACE_BOUND('',#2497,.T.);
#1027=FACE_BOUND('',#2498,.T.);
#1028=FACE_BOUND('',#2499,.T.);
#1029=FACE_BOUND('',#2500,.T.);
#1030=FACE_BOUND('',#2501,.T.);
#1031=FACE_BOUND('',#2502,.T.);
#1032=FACE_BOUND('',#2525,.T.);
#1033=FACE_BOUND('',#2526,.T.);
#1034=FACE_BOUND('',#2528,.T.);
#1035=FACE_BOUND('',#2529,.T.);
#1036=FACE_BOUND('',#2533,.T.);
#1037=FACE_BOUND('',#2534,.T.);
#1038=FACE_BOUND('',#2535,.T.);
#1039=FACE_BOUND('',#2536,.T.);
#1040=FACE_BOUND('',#2537,.T.);
#1041=FACE_BOUND('',#2540,.T.);
#1042=FACE_BOUND('',#2541,.T.);
#1043=FACE_BOUND('',#2542,.T.);
#1044=FACE_BOUND('',#2543,.T.);
#1045=FACE_BOUND('',#2544,.T.);
#1046=FACE_BOUND('',#2548,.T.);
#1047=FACE_BOUND('',#2549,.T.);
#1048=FACE_BOUND('',#2550,.T.);
#1049=FACE_BOUND('',#2551,.T.);
#1050=FACE_BOUND('',#2555,.T.);
#1051=FACE_BOUND('',#2557,.T.);
#1052=FACE_BOUND('',#2563,.T.);
#1053=FACE_BOUND('',#2570,.T.);
#1054=FACE_BOUND('',#2573,.T.);
#1055=FACE_BOUND('',#2579,.T.);
#1056=FACE_BOUND('',#2586,.T.);
#1057=FACE_BOUND('',#2589,.T.);
#1058=FACE_BOUND('',#2593,.T.);
#1059=FACE_BOUND('',#2594,.T.);
#1060=FACE_BOUND('',#2595,.T.);
#1061=FACE_BOUND('',#2596,.T.);
#1062=FACE_BOUND('',#2597,.T.);
#1063=FACE_BOUND('',#2613,.T.);
#1064=FACE_BOUND('',#2614,.T.);
#1065=FACE_BOUND('',#2616,.T.);
#1066=FACE_BOUND('',#2617,.T.);
#1067=FACE_BOUND('',#2621,.T.);
#1068=FACE_BOUND('',#2622,.T.);
#1069=FACE_BOUND('',#2623,.T.);
#1070=FACE_BOUND('',#2624,.T.);
#1071=FACE_BOUND('',#2625,.T.);
#1072=FACE_BOUND('',#2629,.T.);
#1073=FACE_BOUND('',#2630,.T.);
#1074=FACE_BOUND('',#2631,.T.);
#1075=FACE_BOUND('',#2632,.T.);
#1076=FACE_BOUND('',#2636,.T.);
#1077=FACE_BOUND('',#2638,.T.);
#1078=FACE_BOUND('',#2642,.T.);
#1079=FACE_BOUND('',#2644,.T.);
#1080=FACE_BOUND('',#2648,.T.);
#1081=FACE_BOUND('',#2650,.T.);
#1082=FACE_BOUND('',#2654,.T.);
#1083=FACE_BOUND('',#2656,.T.);
#1084=FACE_BOUND('',#2660,.T.);
#1085=FACE_BOUND('',#2662,.T.);
#1086=FACE_BOUND('',#2668,.T.);
#1087=FACE_BOUND('',#2675,.T.);
#1088=FACE_BOUND('',#2678,.T.);
#1089=FACE_BOUND('',#2692,.T.);
#1090=FACE_BOUND('',#2694,.T.);
#1091=FACE_BOUND('',#2703,.T.);
#1092=FACE_BOUND('',#2711,.T.);
#1093=FACE_BOUND('',#2714,.T.);
#1094=FACE_BOUND('',#2718,.T.);
#1095=FACE_BOUND('',#2722,.T.);
#1096=FACE_BOUND('',#2726,.T.);
#1097=FACE_BOUND('',#2737,.T.);
#1098=FACE_BOUND('',#2738,.T.);
#1099=FACE_BOUND('',#2739,.T.);
#1100=FACE_BOUND('',#2740,.T.);
#1101=FACE_BOUND('',#2741,.T.);
#1102=FACE_BOUND('',#2742,.T.);
#1103=FACE_BOUND('',#2744,.T.);
#1104=FACE_BOUND('',#2745,.T.);
#1105=FACE_BOUND('',#2746,.T.);
#1106=FACE_BOUND('',#2747,.T.);
#1107=FACE_BOUND('',#2751,.T.);
#1108=FACE_BOUND('',#2753,.T.);
#1109=FACE_BOUND('',#2757,.T.);
#1110=FACE_BOUND('',#2759,.T.);
#1111=FACE_BOUND('',#2762,.T.);
#1112=FACE_BOUND('',#2766,.T.);
#1113=FACE_BOUND('',#2770,.T.);
#1114=FACE_BOUND('',#2774,.T.);
#1115=FACE_BOUND('',#2785,.T.);
#1116=FACE_BOUND('',#2786,.T.);
#1117=FACE_BOUND('',#2787,.T.);
#1118=FACE_BOUND('',#2788,.T.);
#1119=FACE_BOUND('',#2789,.T.);
#1120=FACE_BOUND('',#2790,.T.);
#1121=FACE_BOUND('',#2792,.T.);
#1122=FACE_BOUND('',#2793,.T.);
#1123=FACE_BOUND('',#2794,.T.);
#1124=FACE_BOUND('',#2795,.T.);
#1125=FACE_BOUND('',#2799,.T.);
#1126=FACE_BOUND('',#2801,.T.);
#1127=FACE_BOUND('',#2805,.T.);
#1128=FACE_BOUND('',#2807,.T.);
#1129=FACE_BOUND('',#2810,.T.);
#1130=FACE_BOUND('',#2814,.T.);
#1131=FACE_BOUND('',#2821,.T.);
#1132=FACE_BOUND('',#2822,.T.);
#1133=FACE_BOUND('',#2824,.T.);
#1134=FACE_BOUND('',#2825,.T.);
#1135=FACE_BOUND('',#2835,.T.);
#1136=FACE_BOUND('',#2836,.T.);
#1137=FACE_BOUND('',#2839,.T.);
#1138=FACE_BOUND('',#2840,.T.);
#1139=FACE_BOUND('',#2847,.T.);
#1140=FACE_BOUND('',#2848,.T.);
#1141=FACE_BOUND('',#2851,.T.);
#1142=FACE_BOUND('',#2852,.T.);
#1143=FACE_BOUND('',#2865,.T.);
#1144=FACE_BOUND('',#2866,.T.);
#1145=FACE_BOUND('',#2867,.T.);
#1146=FACE_BOUND('',#2868,.T.);
#1147=FACE_BOUND('',#2870,.T.);
#1148=FACE_BOUND('',#2871,.T.);
#1149=FACE_BOUND('',#2872,.T.);
#1150=FACE_BOUND('',#2873,.T.);
#1151=FACE_BOUND('',#2879,.T.);
#1152=FACE_BOUND('',#2882,.T.);
#1153=FACE_BOUND('',#2887,.T.);
#1154=FACE_BOUND('',#2892,.T.);
#1155=FACE_BOUND('',#2920,.T.);
#1156=FACE_BOUND('',#2923,.T.);
#1157=FACE_BOUND('',#2926,.T.);
#1158=FACE_BOUND('',#2929,.T.);
#1159=FACE_BOUND('',#2932,.T.);
#1160=FACE_BOUND('',#2943,.T.);
#1161=FACE_BOUND('',#2951,.T.);
#1162=FACE_BOUND('',#2960,.T.);
#1163=FACE_BOUND('',#2963,.T.);
#1164=FACE_BOUND('',#2968,.T.);
#1165=FACE_BOUND('',#2973,.T.);
#1166=FACE_BOUND('',#2998,.T.);
#1167=FACE_BOUND('',#3001,.T.);
#1168=FACE_BOUND('',#3004,.T.);
#1169=FACE_BOUND('',#3007,.T.);
#1170=FACE_BOUND('',#3010,.T.);
#1171=FACE_BOUND('',#3017,.T.);
#1172=FACE_BOUND('',#3033,.T.);
#1173=FACE_BOUND('',#3034,.T.);
#1174=FACE_BOUND('',#3042,.T.);
#1175=FACE_BOUND('',#3043,.T.);
#1176=FACE_BOUND('',#3044,.T.);
#1177=FACE_BOUND('',#3047,.T.);
#1178=FACE_BOUND('',#3049,.T.);
#1179=FACE_BOUND('',#3062,.T.);
#1180=FACE_BOUND('',#3063,.T.);
#1181=FACE_BOUND('',#3064,.T.);
#1182=FACE_BOUND('',#3067,.T.);
#1183=FACE_BOUND('',#3069,.T.);
#1184=FACE_BOUND('',#3070,.T.);
#1185=FACE_BOUND('',#3072,.T.);
#1186=FACE_BOUND('',#3076,.T.);
#1187=FACE_BOUND('',#3077,.T.);
#1188=FACE_BOUND('',#3078,.T.);
#1189=FACE_BOUND('',#3079,.T.);
#1190=FACE_BOUND('',#3080,.T.);
#1191=FACE_BOUND('',#3081,.T.);
#1192=FACE_BOUND('',#3087,.T.);
#1193=FACE_BOUND('',#3089,.T.);
#1194=FACE_BOUND('',#3092,.T.);
#1195=FACE_BOUND('',#3094,.T.);
#1196=FACE_BOUND('',#3095,.T.);
#1197=FACE_BOUND('',#3096,.T.);
#1198=FACE_BOUND('',#3097,.T.);
#1199=FACE_BOUND('',#3098,.T.);
#1200=FACE_BOUND('',#3099,.T.);
#1201=FACE_BOUND('',#3103,.T.);
#1202=FACE_BOUND('',#3105,.T.);
#1203=FACE_BOUND('',#3120,.T.);
#1204=FACE_BOUND('',#3137,.T.);
#1205=FACE_BOUND('',#3143,.T.);
#1206=FACE_BOUND('',#3145,.T.);
#1207=FACE_BOUND('',#3150,.T.);
#1208=FACE_BOUND('',#3154,.T.);
#1209=FACE_BOUND('',#3157,.T.);
#1210=FACE_BOUND('',#3161,.T.);
#1211=FACE_BOUND('',#3163,.T.);
#1212=FACE_BOUND('',#3167,.T.);
#1213=FACE_BOUND('',#3169,.T.);
#1214=FACE_BOUND('',#3179,.T.);
#1215=FACE_BOUND('',#3181,.T.);
#1216=FACE_BOUND('',#3192,.T.);
#1217=FACE_BOUND('',#3193,.T.);
#1218=FACE_BOUND('',#3195,.T.);
#1219=FACE_BOUND('',#3196,.T.);
#1220=FACE_BOUND('',#3198,.T.);
#1221=FACE_BOUND('',#3200,.T.);
#1222=FACE_BOUND('',#3204,.T.);
#1223=FACE_BOUND('',#3205,.T.);
#1224=FACE_BOUND('',#3206,.T.);
#1225=FACE_BOUND('',#3210,.T.);
#1226=FACE_BOUND('',#3211,.T.);
#1227=FACE_BOUND('',#3212,.T.);
#1228=FACE_BOUND('',#3214,.T.);
#1229=FACE_BOUND('',#3216,.T.);
#1230=FACE_BOUND('',#3219,.T.);
#1231=FACE_BOUND('',#3221,.T.);
#1232=FACE_BOUND('',#3224,.T.);
#1233=FACE_BOUND('',#3266,.T.);
#1234=FACE_BOUND('',#3272,.T.);
#1235=FACE_BOUND('',#3276,.T.);
#1236=FACE_BOUND('',#3280,.T.);
#1237=FACE_BOUND('',#3282,.T.);
#1238=FACE_BOUND('',#3286,.T.);
#1239=FACE_BOUND('',#3288,.T.);
#1240=FACE_BOUND('',#3298,.T.);
#1241=FACE_BOUND('',#3300,.T.);
#1242=FACE_BOUND('',#3305,.T.);
#1243=FACE_BOUND('',#3307,.T.);
#1244=FACE_BOUND('',#3309,.T.);
#1245=FACE_BOUND('',#3311,.T.);
#1246=FACE_BOUND('',#3316,.T.);
#1247=FACE_BOUND('',#3318,.T.);
#1248=FACE_BOUND('',#3320,.T.);
#1249=FACE_BOUND('',#3322,.T.);
#1250=FACE_BOUND('',#3326,.T.);
#1251=FACE_BOUND('',#3328,.T.);
#1252=FACE_BOUND('',#3332,.T.);
#1253=FACE_BOUND('',#3334,.T.);
#1254=FACE_BOUND('',#3338,.T.);
#1255=FACE_BOUND('',#3340,.T.);
#1256=FACE_BOUND('',#3345,.T.);
#1257=FACE_BOUND('',#3347,.T.);
#1258=FACE_BOUND('',#3349,.T.);
#1259=FACE_BOUND('',#3351,.T.);
#1260=FACE_BOUND('',#3356,.T.);
#1261=FACE_BOUND('',#3358,.T.);
#1262=FACE_BOUND('',#3360,.T.);
#1263=FACE_BOUND('',#3362,.T.);
#1264=FACE_BOUND('',#3366,.T.);
#1265=FACE_BOUND('',#3367,.T.);
#1266=FACE_BOUND('',#3368,.T.);
#1267=FACE_BOUND('',#3372,.T.);
#1268=FACE_BOUND('',#3373,.T.);
#1269=FACE_BOUND('',#3374,.T.);
#1270=FACE_BOUND('',#3376,.T.);
#1271=FACE_BOUND('',#3378,.T.);
#1272=FACE_BOUND('',#3381,.T.);
#1273=FACE_BOUND('',#3383,.T.);
#1274=FACE_BOUND('',#3386,.T.);
#1275=FACE_BOUND('',#3472,.T.);
#1276=FACE_BOUND('',#3493,.T.);
#1277=PLANE('',#14568);
#1278=PLANE('',#14572);
#1279=PLANE('',#14576);
#1280=PLANE('',#14580);
#1281=PLANE('',#14584);
#1282=PLANE('',#14588);
#1283=PLANE('',#14592);
#1284=PLANE('',#14596);
#1285=PLANE('',#14600);
#1286=PLANE('',#14604);
#1287=PLANE('',#14611);
#1288=PLANE('',#14618);
#1289=PLANE('',#14619);
#1290=PLANE('',#14624);
#1291=PLANE('',#14625);
#1292=PLANE('',#14632);
#1293=PLANE('',#14633);
#1294=PLANE('',#14640);
#1295=PLANE('',#14641);
#1296=PLANE('',#14645);
#1297=PLANE('',#14649);
#1298=PLANE('',#14653);
#1299=PLANE('',#14657);
#1300=PLANE('',#14658);
#1301=PLANE('',#14659);
#1302=PLANE('',#14660);
#1303=PLANE('',#14661);
#1304=PLANE('',#14662);
#1305=PLANE('',#14664);
#1306=PLANE('',#14665);
#1307=PLANE('',#14666);
#1308=PLANE('',#14667);
#1309=PLANE('',#14668);
#1310=PLANE('',#14669);
#1311=PLANE('',#14671);
#1312=PLANE('',#14672);
#1313=PLANE('',#14673);
#1314=PLANE('',#14674);
#1315=PLANE('',#14675);
#1316=PLANE('',#14676);
#1317=PLANE('',#14705);
#1318=PLANE('',#14706);
#1319=PLANE('',#14707);
#1320=PLANE('',#14708);
#1321=PLANE('',#14709);
#1322=PLANE('',#14710);
#1323=PLANE('',#14711);
#1324=PLANE('',#14712);
#1325=PLANE('',#14713);
#1326=PLANE('',#14714);
#1327=PLANE('',#14722);
#1328=PLANE('',#14723);
#1329=PLANE('',#14737);
#1330=PLANE('',#14754);
#1331=PLANE('',#14757);
#1332=PLANE('',#14771);
#1333=PLANE('',#14787);
#1334=PLANE('',#14791);
#1335=PLANE('',#14799);
#1336=PLANE('',#14808);
#1337=PLANE('',#14809);
#1338=PLANE('',#14810);
#1339=PLANE('',#14811);
#1340=PLANE('',#14834);
#1341=PLANE('',#14835);
#1342=PLANE('',#14836);
#1343=PLANE('',#14837);
#1344=PLANE('',#14838);
#1345=PLANE('',#14839);
#1346=PLANE('',#14840);
#1347=PLANE('',#14841);
#1348=PLANE('',#14849);
#1349=PLANE('',#14850);
#1350=PLANE('',#14858);
#1351=PLANE('',#14859);
#1352=PLANE('',#14867);
#1353=PLANE('',#14868);
#1354=PLANE('',#14876);
#1355=PLANE('',#14877);
#1356=PLANE('',#14885);
#1357=PLANE('',#14886);
#1358=PLANE('',#14900);
#1359=PLANE('',#14917);
#1360=PLANE('',#14920);
#1361=PLANE('',#14925);
#1362=PLANE('',#14929);
#1363=PLANE('',#14936);
#1364=PLANE('',#14943);
#1365=PLANE('',#14959);
#1366=PLANE('',#14964);
#1367=PLANE('',#14976);
#1368=PLANE('',#14977);
#1369=PLANE('',#14978);
#1370=PLANE('',#14989);
#1371=PLANE('',#14990);
#1372=PLANE('',#14993);
#1373=PLANE('',#14998);
#1374=PLANE('',#15005);
#1375=PLANE('',#15012);
#1376=PLANE('',#15019);
#1377=PLANE('',#15026);
#1378=PLANE('',#15030);
#1379=PLANE('',#15031);
#1380=PLANE('',#15032);
#1381=PLANE('',#15033);
#1382=PLANE('',#15034);
#1383=PLANE('',#15035);
#1384=PLANE('',#15036);
#1385=PLANE('',#15044);
#1386=PLANE('',#15045);
#1387=PLANE('',#15053);
#1388=PLANE('',#15054);
#1389=PLANE('',#15059);
#1390=PLANE('',#15066);
#1391=PLANE('',#15073);
#1392=PLANE('',#15080);
#1393=PLANE('',#15087);
#1394=PLANE('',#15091);
#1395=PLANE('',#15092);
#1396=PLANE('',#15093);
#1397=PLANE('',#15094);
#1398=PLANE('',#15095);
#1399=PLANE('',#15096);
#1400=PLANE('',#15097);
#1401=PLANE('',#15105);
#1402=PLANE('',#15106);
#1403=PLANE('',#15114);
#1404=PLANE('',#15115);
#1405=PLANE('',#15120);
#1406=PLANE('',#15127);
#1407=PLANE('',#15131);
#1408=PLANE('',#15132);
#1409=PLANE('',#15133);
#1410=PLANE('',#15134);
#1411=PLANE('',#15135);
#1412=PLANE('',#15136);
#1413=PLANE('',#15138);
#1414=PLANE('',#15139);
#1415=PLANE('',#15140);
#1416=PLANE('',#15141);
#1417=PLANE('',#15142);
#1418=PLANE('',#15143);
#1419=PLANE('',#15151);
#1420=PLANE('',#15152);
#1421=PLANE('',#15153);
#1422=PLANE('',#15154);
#1423=PLANE('',#15155);
#1424=PLANE('',#15156);
#1425=PLANE('',#15164);
#1426=PLANE('',#15165);
#1427=PLANE('',#15166);
#1428=PLANE('',#15167);
#1429=PLANE('',#15168);
#1430=PLANE('',#15169);
#1431=PLANE('',#15183);
#1432=PLANE('',#15184);
#1433=PLANE('',#15185);
#1434=PLANE('',#15186);
#1435=PLANE('',#15187);
#1436=PLANE('',#15188);
#1437=PLANE('',#15204);
#1438=PLANE('',#15207);
#1439=PLANE('',#15219);
#1440=PLANE('',#15228);
#1441=PLANE('',#15261);
#1442=PLANE('',#15266);
#1443=PLANE('',#15271);
#1444=PLANE('',#15276);
#1445=PLANE('',#15281);
#1446=PLANE('',#15286);
#1447=PLANE('',#15295);
#1448=PLANE('',#15299);
#1449=PLANE('',#15300);
#1450=PLANE('',#15302);
#1451=PLANE('',#15307);
#1452=PLANE('',#15310);
#1453=PLANE('',#15315);
#1454=PLANE('',#15324);
#1455=PLANE('',#15325);
#1456=PLANE('',#15326);
#1457=PLANE('',#15327);
#1458=PLANE('',#15328);
#1459=PLANE('',#15329);
#1460=PLANE('',#15330);
#1461=PLANE('',#15331);
#1462=PLANE('',#15332);
#1463=PLANE('',#15337);
#1464=PLANE('',#15338);
#1465=PLANE('',#15346);
#1466=PLANE('',#15368);
#1467=PLANE('',#15371);
#1468=PLANE('',#15383);
#1469=PLANE('',#15392);
#1470=PLANE('',#15423);
#1471=PLANE('',#15428);
#1472=PLANE('',#15433);
#1473=PLANE('',#15439);
#1474=PLANE('',#15444);
#1475=PLANE('',#15453);
#1476=PLANE('',#15457);
#1477=PLANE('',#15458);
#1478=PLANE('',#15460);
#1479=PLANE('',#15465);
#1480=PLANE('',#15468);
#1481=PLANE('',#15473);
#1482=PLANE('',#15482);
#1483=PLANE('',#15490);
#1484=PLANE('',#15498);
#1485=PLANE('',#15499);
#1486=PLANE('',#15500);
#1487=PLANE('',#15501);
#1488=PLANE('',#15502);
#1489=PLANE('',#15503);
#1490=PLANE('',#15504);
#1491=PLANE('',#15505);
#1492=PLANE('',#15506);
#1493=PLANE('',#15517);
#1494=PLANE('',#15519);
#1495=PLANE('',#15521);
#1496=PLANE('',#15523);
#1497=PLANE('',#15524);
#1498=PLANE('',#15526);
#1499=PLANE('',#15527);
#1500=PLANE('',#15533);
#1501=PLANE('',#15534);
#1502=PLANE('',#15535);
#1503=PLANE('',#15536);
#1504=PLANE('',#15537);
#1505=PLANE('',#15538);
#1506=PLANE('',#15539);
#1507=PLANE('',#15544);
#1508=PLANE('',#15545);
#1509=PLANE('',#15546);
#1510=PLANE('',#15547);
#1511=PLANE('',#15548);
#1512=PLANE('',#15553);
#1513=PLANE('',#15558);
#1514=PLANE('',#15568);
#1515=PLANE('',#15570);
#1516=PLANE('',#15574);
#1517=PLANE('',#15586);
#1518=PLANE('',#15587);
#1519=PLANE('',#15589);
#1520=PLANE('',#15590);
#1521=PLANE('',#15591);
#1522=PLANE('',#15592);
#1523=PLANE('',#15593);
#1524=PLANE('',#15594);
#1525=PLANE('',#15595);
#1526=PLANE('',#15596);
#1527=PLANE('',#15597);
#1528=PLANE('',#15599);
#1529=PLANE('',#15607);
#1530=PLANE('',#15613);
#1531=PLANE('',#15614);
#1532=PLANE('',#15615);
#1533=PLANE('',#15616);
#1534=PLANE('',#15617);
#1535=PLANE('',#15618);
#1536=PLANE('',#15619);
#1537=PLANE('',#15620);
#1538=PLANE('',#15621);
#1539=PLANE('',#15623);
#1540=PLANE('',#15631);
#1541=PLANE('',#15641);
#1542=PLANE('',#15642);
#1543=PLANE('',#15645);
#1544=PLANE('',#15654);
#1545=PLANE('',#15657);
#1546=PLANE('',#15658);
#1547=PLANE('',#15663);
#1548=PLANE('',#15670);
#1549=PLANE('',#15671);
#1550=PLANE('',#15679);
#1551=PLANE('',#15680);
#1552=PLANE('',#15685);
#1553=PLANE('',#15686);
#1554=PLANE('',#15691);
#1555=PLANE('',#15692);
#1556=PLANE('',#15700);
#1557=PLANE('',#15701);
#1558=PLANE('',#15706);
#1559=PLANE('',#15707);
#1560=PLANE('',#15709);
#1561=PLANE('',#15714);
#1562=PLANE('',#15715);
#1563=PLANE('',#15720);
#1564=PLANE('',#15727);
#1565=PLANE('',#15728);
#1566=PLANE('',#15740);
#1567=PLANE('',#15741);
#1568=PLANE('',#15785);
#1569=PLANE('',#15786);
#1570=PLANE('',#15830);
#1571=PLANE('',#15873);
#1572=PLANE('',#15878);
#1573=PLANE('',#15882);
#1574=PLANE('',#15883);
#1575=PLANE('',#15889);
#1576=PLANE('',#15897);
#1577=PLANE('',#15898);
#1578=PLANE('',#15906);
#1579=PLANE('',#15907);
#1580=PLANE('',#15912);
#1581=PLANE('',#15913);
#1582=PLANE('',#15918);
#1583=PLANE('',#15919);
#1584=PLANE('',#15927);
#1585=PLANE('',#15928);
#1586=PLANE('',#15930);
#1587=PLANE('',#15935);
#1588=PLANE('',#15942);
#1589=PLANE('',#15943);
#1590=PLANE('',#15945);
#1591=PLANE('',#15950);
#1592=PLANE('',#15957);
#1593=PLANE('',#15958);
#1594=PLANE('',#15966);
#1595=PLANE('',#15967);
#1596=PLANE('',#15975);
#1597=PLANE('',#15976);
#1598=PLANE('',#15984);
#1599=PLANE('',#15985);
#1600=PLANE('',#15987);
#1601=PLANE('',#15992);
#1602=PLANE('',#15999);
#1603=PLANE('',#16000);
#1604=PLANE('',#16002);
#1605=PLANE('',#16007);
#1606=PLANE('',#16014);
#1607=PLANE('',#16015);
#1608=PLANE('',#16027);
#1609=PLANE('',#16028);
#1610=PLANE('',#16112);
#1611=PLANE('',#16113);
#1612=PLANE('',#16197);
#1613=PLANE('',#16279);
#1614=PLANE('',#16287);
#1615=PLANE('',#16295);
#1616=PLANE('',#16296);
#1617=PLANE('',#16297);
#1618=PLANE('',#16298);
#1619=PLANE('',#16299);
#1620=PLANE('',#16300);
#1621=PLANE('',#16301);
#1622=PLANE('',#16302);
#1623=PLANE('',#16303);
#1624=PLANE('',#16384);
#1625=PLANE('',#16385);
#1626=PLANE('',#16386);
#1627=PLANE('',#16387);
#1628=PLANE('',#16388);
#1629=PLANE('',#16389);
#1630=PLANE('',#16390);
#1631=PLANE('',#16391);
#1632=PLANE('',#16399);
#1633=FACE_OUTER_BOUND('',#2433,.T.);
#1634=FACE_OUTER_BOUND('',#2434,.T.);
#1635=FACE_OUTER_BOUND('',#2435,.T.);
#1636=FACE_OUTER_BOUND('',#2436,.T.);
#1637=FACE_OUTER_BOUND('',#2437,.T.);
#1638=FACE_OUTER_BOUND('',#2438,.T.);
#1639=FACE_OUTER_BOUND('',#2439,.T.);
#1640=FACE_OUTER_BOUND('',#2440,.T.);
#1641=FACE_OUTER_BOUND('',#2441,.T.);
#1642=FACE_OUTER_BOUND('',#2442,.T.);
#1643=FACE_OUTER_BOUND('',#2443,.T.);
#1644=FACE_OUTER_BOUND('',#2444,.T.);
#1645=FACE_OUTER_BOUND('',#2445,.T.);
#1646=FACE_OUTER_BOUND('',#2446,.T.);
#1647=FACE_OUTER_BOUND('',#2447,.T.);
#1648=FACE_OUTER_BOUND('',#2448,.T.);
#1649=FACE_OUTER_BOUND('',#2449,.T.);
#1650=FACE_OUTER_BOUND('',#2450,.T.);
#1651=FACE_OUTER_BOUND('',#2451,.T.);
#1652=FACE_OUTER_BOUND('',#2452,.T.);
#1653=FACE_OUTER_BOUND('',#2453,.T.);
#1654=FACE_OUTER_BOUND('',#2454,.T.);
#1655=FACE_OUTER_BOUND('',#2455,.T.);
#1656=FACE_OUTER_BOUND('',#2460,.T.);
#1657=FACE_OUTER_BOUND('',#2461,.T.);
#1658=FACE_OUTER_BOUND('',#2462,.T.);
#1659=FACE_OUTER_BOUND('',#2463,.T.);
#1660=FACE_OUTER_BOUND('',#2464,.T.);
#1661=FACE_OUTER_BOUND('',#2465,.T.);
#1662=FACE_OUTER_BOUND('',#2466,.T.);
#1663=FACE_OUTER_BOUND('',#2467,.T.);
#1664=FACE_OUTER_BOUND('',#2468,.T.);
#1665=FACE_OUTER_BOUND('',#2469,.T.);
#1666=FACE_OUTER_BOUND('',#2470,.T.);
#1667=FACE_OUTER_BOUND('',#2471,.T.);
#1668=FACE_OUTER_BOUND('',#2472,.T.);
#1669=FACE_OUTER_BOUND('',#2473,.T.);
#1670=FACE_OUTER_BOUND('',#2474,.T.);
#1671=FACE_OUTER_BOUND('',#2475,.T.);
#1672=FACE_OUTER_BOUND('',#2476,.T.);
#1673=FACE_OUTER_BOUND('',#2477,.T.);
#1674=FACE_OUTER_BOUND('',#2478,.T.);
#1675=FACE_OUTER_BOUND('',#2479,.T.);
#1676=FACE_OUTER_BOUND('',#2480,.T.);
#1677=FACE_OUTER_BOUND('',#2481,.T.);
#1678=FACE_OUTER_BOUND('',#2482,.T.);
#1679=FACE_OUTER_BOUND('',#2483,.T.);
#1680=FACE_OUTER_BOUND('',#2484,.T.);
#1681=FACE_OUTER_BOUND('',#2485,.T.);
#1682=FACE_OUTER_BOUND('',#2486,.T.);
#1683=FACE_OUTER_BOUND('',#2503,.T.);
#1684=FACE_OUTER_BOUND('',#2504,.T.);
#1685=FACE_OUTER_BOUND('',#2505,.T.);
#1686=FACE_OUTER_BOUND('',#2506,.T.);
#1687=FACE_OUTER_BOUND('',#2507,.T.);
#1688=FACE_OUTER_BOUND('',#2508,.T.);
#1689=FACE_OUTER_BOUND('',#2509,.T.);
#1690=FACE_OUTER_BOUND('',#2510,.T.);
#1691=FACE_OUTER_BOUND('',#2511,.T.);
#1692=FACE_OUTER_BOUND('',#2512,.T.);
#1693=FACE_OUTER_BOUND('',#2513,.T.);
#1694=FACE_OUTER_BOUND('',#2514,.T.);
#1695=FACE_OUTER_BOUND('',#2515,.T.);
#1696=FACE_OUTER_BOUND('',#2516,.T.);
#1697=FACE_OUTER_BOUND('',#2517,.T.);
#1698=FACE_OUTER_BOUND('',#2518,.T.);
#1699=FACE_OUTER_BOUND('',#2519,.T.);
#1700=FACE_OUTER_BOUND('',#2520,.T.);
#1701=FACE_OUTER_BOUND('',#2521,.T.);
#1702=FACE_OUTER_BOUND('',#2522,.T.);
#1703=FACE_OUTER_BOUND('',#2523,.T.);
#1704=FACE_OUTER_BOUND('',#2524,.T.);
#1705=FACE_OUTER_BOUND('',#2527,.T.);
#1706=FACE_OUTER_BOUND('',#2530,.T.);
#1707=FACE_OUTER_BOUND('',#2531,.T.);
#1708=FACE_OUTER_BOUND('',#2532,.T.);
#1709=FACE_OUTER_BOUND('',#2538,.T.);
#1710=FACE_OUTER_BOUND('',#2539,.T.);
#1711=FACE_OUTER_BOUND('',#2545,.T.);
#1712=FACE_OUTER_BOUND('',#2546,.T.);
#1713=FACE_OUTER_BOUND('',#2547,.T.);
#1714=FACE_OUTER_BOUND('',#2552,.T.);
#1715=FACE_OUTER_BOUND('',#2553,.T.);
#1716=FACE_OUTER_BOUND('',#2554,.T.);
#1717=FACE_OUTER_BOUND('',#2556,.T.);
#1718=FACE_OUTER_BOUND('',#2558,.T.);
#1719=FACE_OUTER_BOUND('',#2559,.T.);
#1720=FACE_OUTER_BOUND('',#2560,.T.);
#1721=FACE_OUTER_BOUND('',#2561,.T.);
#1722=FACE_OUTER_BOUND('',#2562,.T.);
#1723=FACE_OUTER_BOUND('',#2564,.T.);
#1724=FACE_OUTER_BOUND('',#2565,.T.);
#1725=FACE_OUTER_BOUND('',#2566,.T.);
#1726=FACE_OUTER_BOUND('',#2567,.T.);
#1727=FACE_OUTER_BOUND('',#2568,.T.);
#1728=FACE_OUTER_BOUND('',#2569,.T.);
#1729=FACE_OUTER_BOUND('',#2571,.T.);
#1730=FACE_OUTER_BOUND('',#2572,.T.);
#1731=FACE_OUTER_BOUND('',#2574,.T.);
#1732=FACE_OUTER_BOUND('',#2575,.T.);
#1733=FACE_OUTER_BOUND('',#2576,.T.);
#1734=FACE_OUTER_BOUND('',#2577,.T.);
#1735=FACE_OUTER_BOUND('',#2578,.T.);
#1736=FACE_OUTER_BOUND('',#2580,.T.);
#1737=FACE_OUTER_BOUND('',#2581,.T.);
#1738=FACE_OUTER_BOUND('',#2582,.T.);
#1739=FACE_OUTER_BOUND('',#2583,.T.);
#1740=FACE_OUTER_BOUND('',#2584,.T.);
#1741=FACE_OUTER_BOUND('',#2585,.T.);
#1742=FACE_OUTER_BOUND('',#2587,.T.);
#1743=FACE_OUTER_BOUND('',#2588,.T.);
#1744=FACE_OUTER_BOUND('',#2590,.T.);
#1745=FACE_OUTER_BOUND('',#2591,.T.);
#1746=FACE_OUTER_BOUND('',#2592,.T.);
#1747=FACE_OUTER_BOUND('',#2598,.T.);
#1748=FACE_OUTER_BOUND('',#2599,.T.);
#1749=FACE_OUTER_BOUND('',#2600,.T.);
#1750=FACE_OUTER_BOUND('',#2601,.T.);
#1751=FACE_OUTER_BOUND('',#2602,.T.);
#1752=FACE_OUTER_BOUND('',#2603,.T.);
#1753=FACE_OUTER_BOUND('',#2604,.T.);
#1754=FACE_OUTER_BOUND('',#2605,.T.);
#1755=FACE_OUTER_BOUND('',#2606,.T.);
#1756=FACE_OUTER_BOUND('',#2607,.T.);
#1757=FACE_OUTER_BOUND('',#2608,.T.);
#1758=FACE_OUTER_BOUND('',#2609,.T.);
#1759=FACE_OUTER_BOUND('',#2610,.T.);
#1760=FACE_OUTER_BOUND('',#2611,.T.);
#1761=FACE_OUTER_BOUND('',#2612,.T.);
#1762=FACE_OUTER_BOUND('',#2615,.T.);
#1763=FACE_OUTER_BOUND('',#2618,.T.);
#1764=FACE_OUTER_BOUND('',#2619,.T.);
#1765=FACE_OUTER_BOUND('',#2620,.T.);
#1766=FACE_OUTER_BOUND('',#2626,.T.);
#1767=FACE_OUTER_BOUND('',#2627,.T.);
#1768=FACE_OUTER_BOUND('',#2628,.T.);
#1769=FACE_OUTER_BOUND('',#2633,.T.);
#1770=FACE_OUTER_BOUND('',#2634,.T.);
#1771=FACE_OUTER_BOUND('',#2635,.T.);
#1772=FACE_OUTER_BOUND('',#2637,.T.);
#1773=FACE_OUTER_BOUND('',#2639,.T.);
#1774=FACE_OUTER_BOUND('',#2640,.T.);
#1775=FACE_OUTER_BOUND('',#2641,.T.);
#1776=FACE_OUTER_BOUND('',#2643,.T.);
#1777=FACE_OUTER_BOUND('',#2645,.T.);
#1778=FACE_OUTER_BOUND('',#2646,.T.);
#1779=FACE_OUTER_BOUND('',#2647,.T.);
#1780=FACE_OUTER_BOUND('',#2649,.T.);
#1781=FACE_OUTER_BOUND('',#2651,.T.);
#1782=FACE_OUTER_BOUND('',#2652,.T.);
#1783=FACE_OUTER_BOUND('',#2653,.T.);
#1784=FACE_OUTER_BOUND('',#2655,.T.);
#1785=FACE_OUTER_BOUND('',#2657,.T.);
#1786=FACE_OUTER_BOUND('',#2658,.T.);
#1787=FACE_OUTER_BOUND('',#2659,.T.);
#1788=FACE_OUTER_BOUND('',#2661,.T.);
#1789=FACE_OUTER_BOUND('',#2663,.T.);
#1790=FACE_OUTER_BOUND('',#2664,.T.);
#1791=FACE_OUTER_BOUND('',#2665,.T.);
#1792=FACE_OUTER_BOUND('',#2666,.T.);
#1793=FACE_OUTER_BOUND('',#2667,.T.);
#1794=FACE_OUTER_BOUND('',#2669,.T.);
#1795=FACE_OUTER_BOUND('',#2670,.T.);
#1796=FACE_OUTER_BOUND('',#2671,.T.);
#1797=FACE_OUTER_BOUND('',#2672,.T.);
#1798=FACE_OUTER_BOUND('',#2673,.T.);
#1799=FACE_OUTER_BOUND('',#2674,.T.);
#1800=FACE_OUTER_BOUND('',#2676,.T.);
#1801=FACE_OUTER_BOUND('',#2677,.T.);
#1802=FACE_OUTER_BOUND('',#2679,.T.);
#1803=FACE_OUTER_BOUND('',#2680,.T.);
#1804=FACE_OUTER_BOUND('',#2681,.T.);
#1805=FACE_OUTER_BOUND('',#2682,.T.);
#1806=FACE_OUTER_BOUND('',#2683,.T.);
#1807=FACE_OUTER_BOUND('',#2684,.T.);
#1808=FACE_OUTER_BOUND('',#2685,.T.);
#1809=FACE_OUTER_BOUND('',#2686,.T.);
#1810=FACE_OUTER_BOUND('',#2687,.T.);
#1811=FACE_OUTER_BOUND('',#2688,.T.);
#1812=FACE_OUTER_BOUND('',#2689,.T.);
#1813=FACE_OUTER_BOUND('',#2690,.T.);
#1814=FACE_OUTER_BOUND('',#2691,.T.);
#1815=FACE_OUTER_BOUND('',#2693,.T.);
#1816=FACE_OUTER_BOUND('',#2695,.T.);
#1817=FACE_OUTER_BOUND('',#2696,.T.);
#1818=FACE_OUTER_BOUND('',#2697,.T.);
#1819=FACE_OUTER_BOUND('',#2698,.T.);
#1820=FACE_OUTER_BOUND('',#2699,.T.);
#1821=FACE_OUTER_BOUND('',#2700,.T.);
#1822=FACE_OUTER_BOUND('',#2701,.T.);
#1823=FACE_OUTER_BOUND('',#2702,.T.);
#1824=FACE_OUTER_BOUND('',#2704,.T.);
#1825=FACE_OUTER_BOUND('',#2705,.T.);
#1826=FACE_OUTER_BOUND('',#2706,.T.);
#1827=FACE_OUTER_BOUND('',#2707,.T.);
#1828=FACE_OUTER_BOUND('',#2708,.T.);
#1829=FACE_OUTER_BOUND('',#2709,.T.);
#1830=FACE_OUTER_BOUND('',#2710,.T.);
#1831=FACE_OUTER_BOUND('',#2712,.T.);
#1832=FACE_OUTER_BOUND('',#2713,.T.);
#1833=FACE_OUTER_BOUND('',#2715,.T.);
#1834=FACE_OUTER_BOUND('',#2716,.T.);
#1835=FACE_OUTER_BOUND('',#2717,.T.);
#1836=FACE_OUTER_BOUND('',#2719,.T.);
#1837=FACE_OUTER_BOUND('',#2720,.T.);
#1838=FACE_OUTER_BOUND('',#2721,.T.);
#1839=FACE_OUTER_BOUND('',#2723,.T.);
#1840=FACE_OUTER_BOUND('',#2724,.T.);
#1841=FACE_OUTER_BOUND('',#2725,.T.);
#1842=FACE_OUTER_BOUND('',#2727,.T.);
#1843=FACE_OUTER_BOUND('',#2728,.T.);
#1844=FACE_OUTER_BOUND('',#2729,.T.);
#1845=FACE_OUTER_BOUND('',#2730,.T.);
#1846=FACE_OUTER_BOUND('',#2731,.T.);
#1847=FACE_OUTER_BOUND('',#2732,.T.);
#1848=FACE_OUTER_BOUND('',#2733,.T.);
#1849=FACE_OUTER_BOUND('',#2734,.T.);
#1850=FACE_OUTER_BOUND('',#2735,.T.);
#1851=FACE_OUTER_BOUND('',#2736,.T.);
#1852=FACE_OUTER_BOUND('',#2743,.T.);
#1853=FACE_OUTER_BOUND('',#2748,.T.);
#1854=FACE_OUTER_BOUND('',#2749,.T.);
#1855=FACE_OUTER_BOUND('',#2750,.T.);
#1856=FACE_OUTER_BOUND('',#2752,.T.);
#1857=FACE_OUTER_BOUND('',#2754,.T.);
#1858=FACE_OUTER_BOUND('',#2755,.T.);
#1859=FACE_OUTER_BOUND('',#2756,.T.);
#1860=FACE_OUTER_BOUND('',#2758,.T.);
#1861=FACE_OUTER_BOUND('',#2760,.T.);
#1862=FACE_OUTER_BOUND('',#2761,.T.);
#1863=FACE_OUTER_BOUND('',#2763,.T.);
#1864=FACE_OUTER_BOUND('',#2764,.T.);
#1865=FACE_OUTER_BOUND('',#2765,.T.);
#1866=FACE_OUTER_BOUND('',#2767,.T.);
#1867=FACE_OUTER_BOUND('',#2768,.T.);
#1868=FACE_OUTER_BOUND('',#2769,.T.);
#1869=FACE_OUTER_BOUND('',#2771,.T.);
#1870=FACE_OUTER_BOUND('',#2772,.T.);
#1871=FACE_OUTER_BOUND('',#2773,.T.);
#1872=FACE_OUTER_BOUND('',#2775,.T.);
#1873=FACE_OUTER_BOUND('',#2776,.T.);
#1874=FACE_OUTER_BOUND('',#2777,.T.);
#1875=FACE_OUTER_BOUND('',#2778,.T.);
#1876=FACE_OUTER_BOUND('',#2779,.T.);
#1877=FACE_OUTER_BOUND('',#2780,.T.);
#1878=FACE_OUTER_BOUND('',#2781,.T.);
#1879=FACE_OUTER_BOUND('',#2782,.T.);
#1880=FACE_OUTER_BOUND('',#2783,.T.);
#1881=FACE_OUTER_BOUND('',#2784,.T.);
#1882=FACE_OUTER_BOUND('',#2791,.T.);
#1883=FACE_OUTER_BOUND('',#2796,.T.);
#1884=FACE_OUTER_BOUND('',#2797,.T.);
#1885=FACE_OUTER_BOUND('',#2798,.T.);
#1886=FACE_OUTER_BOUND('',#2800,.T.);
#1887=FACE_OUTER_BOUND('',#2802,.T.);
#1888=FACE_OUTER_BOUND('',#2803,.T.);
#1889=FACE_OUTER_BOUND('',#2804,.T.);
#1890=FACE_OUTER_BOUND('',#2806,.T.);
#1891=FACE_OUTER_BOUND('',#2808,.T.);
#1892=FACE_OUTER_BOUND('',#2809,.T.);
#1893=FACE_OUTER_BOUND('',#2811,.T.);
#1894=FACE_OUTER_BOUND('',#2812,.T.);
#1895=FACE_OUTER_BOUND('',#2813,.T.);
#1896=FACE_OUTER_BOUND('',#2815,.T.);
#1897=FACE_OUTER_BOUND('',#2816,.T.);
#1898=FACE_OUTER_BOUND('',#2817,.T.);
#1899=FACE_OUTER_BOUND('',#2818,.T.);
#1900=FACE_OUTER_BOUND('',#2819,.T.);
#1901=FACE_OUTER_BOUND('',#2820,.T.);
#1902=FACE_OUTER_BOUND('',#2823,.T.);
#1903=FACE_OUTER_BOUND('',#2826,.T.);
#1904=FACE_OUTER_BOUND('',#2827,.T.);
#1905=FACE_OUTER_BOUND('',#2828,.T.);
#1906=FACE_OUTER_BOUND('',#2829,.T.);
#1907=FACE_OUTER_BOUND('',#2830,.T.);
#1908=FACE_OUTER_BOUND('',#2831,.T.);
#1909=FACE_OUTER_BOUND('',#2832,.T.);
#1910=FACE_OUTER_BOUND('',#2833,.T.);
#1911=FACE_OUTER_BOUND('',#2834,.T.);
#1912=FACE_OUTER_BOUND('',#2837,.T.);
#1913=FACE_OUTER_BOUND('',#2838,.T.);
#1914=FACE_OUTER_BOUND('',#2841,.T.);
#1915=FACE_OUTER_BOUND('',#2842,.T.);
#1916=FACE_OUTER_BOUND('',#2843,.T.);
#1917=FACE_OUTER_BOUND('',#2844,.T.);
#1918=FACE_OUTER_BOUND('',#2845,.T.);
#1919=FACE_OUTER_BOUND('',#2846,.T.);
#1920=FACE_OUTER_BOUND('',#2849,.T.);
#1921=FACE_OUTER_BOUND('',#2850,.T.);
#1922=FACE_OUTER_BOUND('',#2853,.T.);
#1923=FACE_OUTER_BOUND('',#2854,.T.);
#1924=FACE_OUTER_BOUND('',#2855,.T.);
#1925=FACE_OUTER_BOUND('',#2856,.T.);
#1926=FACE_OUTER_BOUND('',#2857,.T.);
#1927=FACE_OUTER_BOUND('',#2858,.T.);
#1928=FACE_OUTER_BOUND('',#2859,.T.);
#1929=FACE_OUTER_BOUND('',#2860,.T.);
#1930=FACE_OUTER_BOUND('',#2861,.T.);
#1931=FACE_OUTER_BOUND('',#2862,.T.);
#1932=FACE_OUTER_BOUND('',#2863,.T.);
#1933=FACE_OUTER_BOUND('',#2864,.T.);
#1934=FACE_OUTER_BOUND('',#2869,.T.);
#1935=FACE_OUTER_BOUND('',#2874,.T.);
#1936=FACE_OUTER_BOUND('',#2875,.T.);
#1937=FACE_OUTER_BOUND('',#2876,.T.);
#1938=FACE_OUTER_BOUND('',#2877,.T.);
#1939=FACE_OUTER_BOUND('',#2878,.T.);
#1940=FACE_OUTER_BOUND('',#2880,.T.);
#1941=FACE_OUTER_BOUND('',#2881,.T.);
#1942=FACE_OUTER_BOUND('',#2883,.T.);
#1943=FACE_OUTER_BOUND('',#2884,.T.);
#1944=FACE_OUTER_BOUND('',#2885,.T.);
#1945=FACE_OUTER_BOUND('',#2886,.T.);
#1946=FACE_OUTER_BOUND('',#2888,.T.);
#1947=FACE_OUTER_BOUND('',#2889,.T.);
#1948=FACE_OUTER_BOUND('',#2890,.T.);
#1949=FACE_OUTER_BOUND('',#2891,.T.);
#1950=FACE_OUTER_BOUND('',#2893,.T.);
#1951=FACE_OUTER_BOUND('',#2894,.T.);
#1952=FACE_OUTER_BOUND('',#2895,.T.);
#1953=FACE_OUTER_BOUND('',#2896,.T.);
#1954=FACE_OUTER_BOUND('',#2897,.T.);
#1955=FACE_OUTER_BOUND('',#2898,.T.);
#1956=FACE_OUTER_BOUND('',#2899,.T.);
#1957=FACE_OUTER_BOUND('',#2900,.T.);
#1958=FACE_OUTER_BOUND('',#2901,.T.);
#1959=FACE_OUTER_BOUND('',#2902,.T.);
#1960=FACE_OUTER_BOUND('',#2903,.T.);
#1961=FACE_OUTER_BOUND('',#2904,.T.);
#1962=FACE_OUTER_BOUND('',#2905,.T.);
#1963=FACE_OUTER_BOUND('',#2906,.T.);
#1964=FACE_OUTER_BOUND('',#2907,.T.);
#1965=FACE_OUTER_BOUND('',#2908,.T.);
#1966=FACE_OUTER_BOUND('',#2909,.T.);
#1967=FACE_OUTER_BOUND('',#2910,.T.);
#1968=FACE_OUTER_BOUND('',#2911,.T.);
#1969=FACE_OUTER_BOUND('',#2912,.T.);
#1970=FACE_OUTER_BOUND('',#2913,.T.);
#1971=FACE_OUTER_BOUND('',#2914,.T.);
#1972=FACE_OUTER_BOUND('',#2915,.T.);
#1973=FACE_OUTER_BOUND('',#2916,.T.);
#1974=FACE_OUTER_BOUND('',#2917,.T.);
#1975=FACE_OUTER_BOUND('',#2918,.T.);
#1976=FACE_OUTER_BOUND('',#2919,.T.);
#1977=FACE_OUTER_BOUND('',#2921,.T.);
#1978=FACE_OUTER_BOUND('',#2922,.T.);
#1979=FACE_OUTER_BOUND('',#2924,.T.);
#1980=FACE_OUTER_BOUND('',#2925,.T.);
#1981=FACE_OUTER_BOUND('',#2927,.T.);
#1982=FACE_OUTER_BOUND('',#2928,.T.);
#1983=FACE_OUTER_BOUND('',#2930,.T.);
#1984=FACE_OUTER_BOUND('',#2931,.T.);
#1985=FACE_OUTER_BOUND('',#2933,.T.);
#1986=FACE_OUTER_BOUND('',#2934,.T.);
#1987=FACE_OUTER_BOUND('',#2935,.T.);
#1988=FACE_OUTER_BOUND('',#2936,.T.);
#1989=FACE_OUTER_BOUND('',#2937,.T.);
#1990=FACE_OUTER_BOUND('',#2938,.T.);
#1991=FACE_OUTER_BOUND('',#2939,.T.);
#1992=FACE_OUTER_BOUND('',#2940,.T.);
#1993=FACE_OUTER_BOUND('',#2941,.T.);
#1994=FACE_OUTER_BOUND('',#2942,.T.);
#1995=FACE_OUTER_BOUND('',#2944,.T.);
#1996=FACE_OUTER_BOUND('',#2945,.T.);
#1997=FACE_OUTER_BOUND('',#2946,.T.);
#1998=FACE_OUTER_BOUND('',#2947,.T.);
#1999=FACE_OUTER_BOUND('',#2948,.T.);
#2000=FACE_OUTER_BOUND('',#2949,.T.);
#2001=FACE_OUTER_BOUND('',#2950,.T.);
#2002=FACE_OUTER_BOUND('',#2952,.T.);
#2003=FACE_OUTER_BOUND('',#2953,.T.);
#2004=FACE_OUTER_BOUND('',#2954,.T.);
#2005=FACE_OUTER_BOUND('',#2955,.T.);
#2006=FACE_OUTER_BOUND('',#2956,.T.);
#2007=FACE_OUTER_BOUND('',#2957,.T.);
#2008=FACE_OUTER_BOUND('',#2958,.T.);
#2009=FACE_OUTER_BOUND('',#2959,.T.);
#2010=FACE_OUTER_BOUND('',#2961,.T.);
#2011=FACE_OUTER_BOUND('',#2962,.T.);
#2012=FACE_OUTER_BOUND('',#2964,.T.);
#2013=FACE_OUTER_BOUND('',#2965,.T.);
#2014=FACE_OUTER_BOUND('',#2966,.T.);
#2015=FACE_OUTER_BOUND('',#2967,.T.);
#2016=FACE_OUTER_BOUND('',#2969,.T.);
#2017=FACE_OUTER_BOUND('',#2970,.T.);
#2018=FACE_OUTER_BOUND('',#2971,.T.);
#2019=FACE_OUTER_BOUND('',#2972,.T.);
#2020=FACE_OUTER_BOUND('',#2974,.T.);
#2021=FACE_OUTER_BOUND('',#2975,.T.);
#2022=FACE_OUTER_BOUND('',#2976,.T.);
#2023=FACE_OUTER_BOUND('',#2977,.T.);
#2024=FACE_OUTER_BOUND('',#2978,.T.);
#2025=FACE_OUTER_BOUND('',#2979,.T.);
#2026=FACE_OUTER_BOUND('',#2980,.T.);
#2027=FACE_OUTER_BOUND('',#2981,.T.);
#2028=FACE_OUTER_BOUND('',#2982,.T.);
#2029=FACE_OUTER_BOUND('',#2983,.T.);
#2030=FACE_OUTER_BOUND('',#2984,.T.);
#2031=FACE_OUTER_BOUND('',#2985,.T.);
#2032=FACE_OUTER_BOUND('',#2986,.T.);
#2033=FACE_OUTER_BOUND('',#2987,.T.);
#2034=FACE_OUTER_BOUND('',#2988,.T.);
#2035=FACE_OUTER_BOUND('',#2989,.T.);
#2036=FACE_OUTER_BOUND('',#2990,.T.);
#2037=FACE_OUTER_BOUND('',#2991,.T.);
#2038=FACE_OUTER_BOUND('',#2992,.T.);
#2039=FACE_OUTER_BOUND('',#2993,.T.);
#2040=FACE_OUTER_BOUND('',#2994,.T.);
#2041=FACE_OUTER_BOUND('',#2995,.T.);
#2042=FACE_OUTER_BOUND('',#2996,.T.);
#2043=FACE_OUTER_BOUND('',#2997,.T.);
#2044=FACE_OUTER_BOUND('',#2999,.T.);
#2045=FACE_OUTER_BOUND('',#3000,.T.);
#2046=FACE_OUTER_BOUND('',#3002,.T.);
#2047=FACE_OUTER_BOUND('',#3003,.T.);
#2048=FACE_OUTER_BOUND('',#3005,.T.);
#2049=FACE_OUTER_BOUND('',#3006,.T.);
#2050=FACE_OUTER_BOUND('',#3008,.T.);
#2051=FACE_OUTER_BOUND('',#3009,.T.);
#2052=FACE_OUTER_BOUND('',#3011,.T.);
#2053=FACE_OUTER_BOUND('',#3012,.T.);
#2054=FACE_OUTER_BOUND('',#3013,.T.);
#2055=FACE_OUTER_BOUND('',#3014,.T.);
#2056=FACE_OUTER_BOUND('',#3015,.T.);
#2057=FACE_OUTER_BOUND('',#3016,.T.);
#2058=FACE_OUTER_BOUND('',#3018,.T.);
#2059=FACE_OUTER_BOUND('',#3019,.T.);
#2060=FACE_OUTER_BOUND('',#3020,.T.);
#2061=FACE_OUTER_BOUND('',#3021,.T.);
#2062=FACE_OUTER_BOUND('',#3022,.T.);
#2063=FACE_OUTER_BOUND('',#3023,.T.);
#2064=FACE_OUTER_BOUND('',#3024,.T.);
#2065=FACE_OUTER_BOUND('',#3025,.T.);
#2066=FACE_OUTER_BOUND('',#3026,.T.);
#2067=FACE_OUTER_BOUND('',#3027,.T.);
#2068=FACE_OUTER_BOUND('',#3028,.T.);
#2069=FACE_OUTER_BOUND('',#3029,.T.);
#2070=FACE_OUTER_BOUND('',#3030,.T.);
#2071=FACE_OUTER_BOUND('',#3031,.T.);
#2072=FACE_OUTER_BOUND('',#3032,.T.);
#2073=FACE_OUTER_BOUND('',#3035,.T.);
#2074=FACE_OUTER_BOUND('',#3036,.T.);
#2075=FACE_OUTER_BOUND('',#3037,.T.);
#2076=FACE_OUTER_BOUND('',#3038,.T.);
#2077=FACE_OUTER_BOUND('',#3039,.T.);
#2078=FACE_OUTER_BOUND('',#3040,.T.);
#2079=FACE_OUTER_BOUND('',#3041,.T.);
#2080=FACE_OUTER_BOUND('',#3045,.T.);
#2081=FACE_OUTER_BOUND('',#3046,.T.);
#2082=FACE_OUTER_BOUND('',#3048,.T.);
#2083=FACE_OUTER_BOUND('',#3050,.T.);
#2084=FACE_OUTER_BOUND('',#3051,.T.);
#2085=FACE_OUTER_BOUND('',#3052,.T.);
#2086=FACE_OUTER_BOUND('',#3053,.T.);
#2087=FACE_OUTER_BOUND('',#3054,.T.);
#2088=FACE_OUTER_BOUND('',#3055,.T.);
#2089=FACE_OUTER_BOUND('',#3056,.T.);
#2090=FACE_OUTER_BOUND('',#3057,.T.);
#2091=FACE_OUTER_BOUND('',#3058,.T.);
#2092=FACE_OUTER_BOUND('',#3059,.T.);
#2093=FACE_OUTER_BOUND('',#3060,.T.);
#2094=FACE_OUTER_BOUND('',#3061,.T.);
#2095=FACE_OUTER_BOUND('',#3065,.T.);
#2096=FACE_OUTER_BOUND('',#3066,.T.);
#2097=FACE_OUTER_BOUND('',#3068,.T.);
#2098=FACE_OUTER_BOUND('',#3071,.T.);
#2099=FACE_OUTER_BOUND('',#3073,.T.);
#2100=FACE_OUTER_BOUND('',#3074,.T.);
#2101=FACE_OUTER_BOUND('',#3075,.T.);
#2102=FACE_OUTER_BOUND('',#3082,.T.);
#2103=FACE_OUTER_BOUND('',#3083,.T.);
#2104=FACE_OUTER_BOUND('',#3084,.T.);
#2105=FACE_OUTER_BOUND('',#3085,.T.);
#2106=FACE_OUTER_BOUND('',#3086,.T.);
#2107=FACE_OUTER_BOUND('',#3088,.T.);
#2108=FACE_OUTER_BOUND('',#3090,.T.);
#2109=FACE_OUTER_BOUND('',#3091,.T.);
#2110=FACE_OUTER_BOUND('',#3093,.T.);
#2111=FACE_OUTER_BOUND('',#3100,.T.);
#2112=FACE_OUTER_BOUND('',#3101,.T.);
#2113=FACE_OUTER_BOUND('',#3102,.T.);
#2114=FACE_OUTER_BOUND('',#3104,.T.);
#2115=FACE_OUTER_BOUND('',#3106,.T.);
#2116=FACE_OUTER_BOUND('',#3107,.T.);
#2117=FACE_OUTER_BOUND('',#3108,.T.);
#2118=FACE_OUTER_BOUND('',#3109,.T.);
#2119=FACE_OUTER_BOUND('',#3110,.T.);
#2120=FACE_OUTER_BOUND('',#3111,.T.);
#2121=FACE_OUTER_BOUND('',#3112,.T.);
#2122=FACE_OUTER_BOUND('',#3113,.T.);
#2123=FACE_OUTER_BOUND('',#3114,.T.);
#2124=FACE_OUTER_BOUND('',#3115,.T.);
#2125=FACE_OUTER_BOUND('',#3116,.T.);
#2126=FACE_OUTER_BOUND('',#3117,.T.);
#2127=FACE_OUTER_BOUND('',#3118,.T.);
#2128=FACE_OUTER_BOUND('',#3119,.T.);
#2129=FACE_OUTER_BOUND('',#3121,.T.);
#2130=FACE_OUTER_BOUND('',#3122,.T.);
#2131=FACE_OUTER_BOUND('',#3123,.T.);
#2132=FACE_OUTER_BOUND('',#3124,.T.);
#2133=FACE_OUTER_BOUND('',#3125,.T.);
#2134=FACE_OUTER_BOUND('',#3126,.T.);
#2135=FACE_OUTER_BOUND('',#3127,.T.);
#2136=FACE_OUTER_BOUND('',#3128,.T.);
#2137=FACE_OUTER_BOUND('',#3129,.T.);
#2138=FACE_OUTER_BOUND('',#3130,.T.);
#2139=FACE_OUTER_BOUND('',#3131,.T.);
#2140=FACE_OUTER_BOUND('',#3132,.T.);
#2141=FACE_OUTER_BOUND('',#3133,.T.);
#2142=FACE_OUTER_BOUND('',#3134,.T.);
#2143=FACE_OUTER_BOUND('',#3135,.T.);
#2144=FACE_OUTER_BOUND('',#3136,.T.);
#2145=FACE_OUTER_BOUND('',#3138,.T.);
#2146=FACE_OUTER_BOUND('',#3139,.T.);
#2147=FACE_OUTER_BOUND('',#3140,.T.);
#2148=FACE_OUTER_BOUND('',#3141,.T.);
#2149=FACE_OUTER_BOUND('',#3142,.T.);
#2150=FACE_OUTER_BOUND('',#3144,.T.);
#2151=FACE_OUTER_BOUND('',#3146,.T.);
#2152=FACE_OUTER_BOUND('',#3147,.T.);
#2153=FACE_OUTER_BOUND('',#3148,.T.);
#2154=FACE_OUTER_BOUND('',#3149,.T.);
#2155=FACE_OUTER_BOUND('',#3151,.T.);
#2156=FACE_OUTER_BOUND('',#3152,.T.);
#2157=FACE_OUTER_BOUND('',#3153,.T.);
#2158=FACE_OUTER_BOUND('',#3155,.T.);
#2159=FACE_OUTER_BOUND('',#3156,.T.);
#2160=FACE_OUTER_BOUND('',#3158,.T.);
#2161=FACE_OUTER_BOUND('',#3159,.T.);
#2162=FACE_OUTER_BOUND('',#3160,.T.);
#2163=FACE_OUTER_BOUND('',#3162,.T.);
#2164=FACE_OUTER_BOUND('',#3164,.T.);
#2165=FACE_OUTER_BOUND('',#3165,.T.);
#2166=FACE_OUTER_BOUND('',#3166,.T.);
#2167=FACE_OUTER_BOUND('',#3168,.T.);
#2168=FACE_OUTER_BOUND('',#3170,.T.);
#2169=FACE_OUTER_BOUND('',#3171,.T.);
#2170=FACE_OUTER_BOUND('',#3172,.T.);
#2171=FACE_OUTER_BOUND('',#3173,.T.);
#2172=FACE_OUTER_BOUND('',#3174,.T.);
#2173=FACE_OUTER_BOUND('',#3175,.T.);
#2174=FACE_OUTER_BOUND('',#3176,.T.);
#2175=FACE_OUTER_BOUND('',#3177,.T.);
#2176=FACE_OUTER_BOUND('',#3178,.T.);
#2177=FACE_OUTER_BOUND('',#3180,.T.);
#2178=FACE_OUTER_BOUND('',#3182,.T.);
#2179=FACE_OUTER_BOUND('',#3183,.T.);
#2180=FACE_OUTER_BOUND('',#3184,.T.);
#2181=FACE_OUTER_BOUND('',#3185,.T.);
#2182=FACE_OUTER_BOUND('',#3186,.T.);
#2183=FACE_OUTER_BOUND('',#3187,.T.);
#2184=FACE_OUTER_BOUND('',#3188,.T.);
#2185=FACE_OUTER_BOUND('',#3189,.T.);
#2186=FACE_OUTER_BOUND('',#3190,.T.);
#2187=FACE_OUTER_BOUND('',#3191,.T.);
#2188=FACE_OUTER_BOUND('',#3194,.T.);
#2189=FACE_OUTER_BOUND('',#3197,.T.);
#2190=FACE_OUTER_BOUND('',#3199,.T.);
#2191=FACE_OUTER_BOUND('',#3201,.T.);
#2192=FACE_OUTER_BOUND('',#3202,.T.);
#2193=FACE_OUTER_BOUND('',#3203,.T.);
#2194=FACE_OUTER_BOUND('',#3207,.T.);
#2195=FACE_OUTER_BOUND('',#3208,.T.);
#2196=FACE_OUTER_BOUND('',#3209,.T.);
#2197=FACE_OUTER_BOUND('',#3213,.T.);
#2198=FACE_OUTER_BOUND('',#3215,.T.);
#2199=FACE_OUTER_BOUND('',#3217,.T.);
#2200=FACE_OUTER_BOUND('',#3218,.T.);
#2201=FACE_OUTER_BOUND('',#3220,.T.);
#2202=FACE_OUTER_BOUND('',#3222,.T.);
#2203=FACE_OUTER_BOUND('',#3223,.T.);
#2204=FACE_OUTER_BOUND('',#3225,.T.);
#2205=FACE_OUTER_BOUND('',#3226,.T.);
#2206=FACE_OUTER_BOUND('',#3227,.T.);
#2207=FACE_OUTER_BOUND('',#3228,.T.);
#2208=FACE_OUTER_BOUND('',#3229,.T.);
#2209=FACE_OUTER_BOUND('',#3230,.T.);
#2210=FACE_OUTER_BOUND('',#3231,.T.);
#2211=FACE_OUTER_BOUND('',#3232,.T.);
#2212=FACE_OUTER_BOUND('',#3233,.T.);
#2213=FACE_OUTER_BOUND('',#3234,.T.);
#2214=FACE_OUTER_BOUND('',#3235,.T.);
#2215=FACE_OUTER_BOUND('',#3236,.T.);
#2216=FACE_OUTER_BOUND('',#3237,.T.);
#2217=FACE_OUTER_BOUND('',#3238,.T.);
#2218=FACE_OUTER_BOUND('',#3239,.T.);
#2219=FACE_OUTER_BOUND('',#3240,.T.);
#2220=FACE_OUTER_BOUND('',#3241,.T.);
#2221=FACE_OUTER_BOUND('',#3242,.T.);
#2222=FACE_OUTER_BOUND('',#3243,.T.);
#2223=FACE_OUTER_BOUND('',#3244,.T.);
#2224=FACE_OUTER_BOUND('',#3245,.T.);
#2225=FACE_OUTER_BOUND('',#3246,.T.);
#2226=FACE_OUTER_BOUND('',#3247,.T.);
#2227=FACE_OUTER_BOUND('',#3248,.T.);
#2228=FACE_OUTER_BOUND('',#3249,.T.);
#2229=FACE_OUTER_BOUND('',#3250,.T.);
#2230=FACE_OUTER_BOUND('',#3251,.T.);
#2231=FACE_OUTER_BOUND('',#3252,.T.);
#2232=FACE_OUTER_BOUND('',#3253,.T.);
#2233=FACE_OUTER_BOUND('',#3254,.T.);
#2234=FACE_OUTER_BOUND('',#3255,.T.);
#2235=FACE_OUTER_BOUND('',#3256,.T.);
#2236=FACE_OUTER_BOUND('',#3257,.T.);
#2237=FACE_OUTER_BOUND('',#3258,.T.);
#2238=FACE_OUTER_BOUND('',#3259,.T.);
#2239=FACE_OUTER_BOUND('',#3260,.T.);
#2240=FACE_OUTER_BOUND('',#3261,.T.);
#2241=FACE_OUTER_BOUND('',#3262,.T.);
#2242=FACE_OUTER_BOUND('',#3263,.T.);
#2243=FACE_OUTER_BOUND('',#3264,.T.);
#2244=FACE_OUTER_BOUND('',#3265,.T.);
#2245=FACE_OUTER_BOUND('',#3267,.T.);
#2246=FACE_OUTER_BOUND('',#3268,.T.);
#2247=FACE_OUTER_BOUND('',#3269,.T.);
#2248=FACE_OUTER_BOUND('',#3270,.T.);
#2249=FACE_OUTER_BOUND('',#3271,.T.);
#2250=FACE_OUTER_BOUND('',#3273,.T.);
#2251=FACE_OUTER_BOUND('',#3274,.T.);
#2252=FACE_OUTER_BOUND('',#3275,.T.);
#2253=FACE_OUTER_BOUND('',#3277,.T.);
#2254=FACE_OUTER_BOUND('',#3278,.T.);
#2255=FACE_OUTER_BOUND('',#3279,.T.);
#2256=FACE_OUTER_BOUND('',#3281,.T.);
#2257=FACE_OUTER_BOUND('',#3283,.T.);
#2258=FACE_OUTER_BOUND('',#3284,.T.);
#2259=FACE_OUTER_BOUND('',#3285,.T.);
#2260=FACE_OUTER_BOUND('',#3287,.T.);
#2261=FACE_OUTER_BOUND('',#3289,.T.);
#2262=FACE_OUTER_BOUND('',#3290,.T.);
#2263=FACE_OUTER_BOUND('',#3291,.T.);
#2264=FACE_OUTER_BOUND('',#3292,.T.);
#2265=FACE_OUTER_BOUND('',#3293,.T.);
#2266=FACE_OUTER_BOUND('',#3294,.T.);
#2267=FACE_OUTER_BOUND('',#3295,.T.);
#2268=FACE_OUTER_BOUND('',#3296,.T.);
#2269=FACE_OUTER_BOUND('',#3297,.T.);
#2270=FACE_OUTER_BOUND('',#3299,.T.);
#2271=FACE_OUTER_BOUND('',#3301,.T.);
#2272=FACE_OUTER_BOUND('',#3302,.T.);
#2273=FACE_OUTER_BOUND('',#3303,.T.);
#2274=FACE_OUTER_BOUND('',#3304,.T.);
#2275=FACE_OUTER_BOUND('',#3306,.T.);
#2276=FACE_OUTER_BOUND('',#3308,.T.);
#2277=FACE_OUTER_BOUND('',#3310,.T.);
#2278=FACE_OUTER_BOUND('',#3312,.T.);
#2279=FACE_OUTER_BOUND('',#3313,.T.);
#2280=FACE_OUTER_BOUND('',#3314,.T.);
#2281=FACE_OUTER_BOUND('',#3315,.T.);
#2282=FACE_OUTER_BOUND('',#3317,.T.);
#2283=FACE_OUTER_BOUND('',#3319,.T.);
#2284=FACE_OUTER_BOUND('',#3321,.T.);
#2285=FACE_OUTER_BOUND('',#3323,.T.);
#2286=FACE_OUTER_BOUND('',#3324,.T.);
#2287=FACE_OUTER_BOUND('',#3325,.T.);
#2288=FACE_OUTER_BOUND('',#3327,.T.);
#2289=FACE_OUTER_BOUND('',#3329,.T.);
#2290=FACE_OUTER_BOUND('',#3330,.T.);
#2291=FACE_OUTER_BOUND('',#3331,.T.);
#2292=FACE_OUTER_BOUND('',#3333,.T.);
#2293=FACE_OUTER_BOUND('',#3335,.T.);
#2294=FACE_OUTER_BOUND('',#3336,.T.);
#2295=FACE_OUTER_BOUND('',#3337,.T.);
#2296=FACE_OUTER_BOUND('',#3339,.T.);
#2297=FACE_OUTER_BOUND('',#3341,.T.);
#2298=FACE_OUTER_BOUND('',#3342,.T.);
#2299=FACE_OUTER_BOUND('',#3343,.T.);
#2300=FACE_OUTER_BOUND('',#3344,.T.);
#2301=FACE_OUTER_BOUND('',#3346,.T.);
#2302=FACE_OUTER_BOUND('',#3348,.T.);
#2303=FACE_OUTER_BOUND('',#3350,.T.);
#2304=FACE_OUTER_BOUND('',#3352,.T.);
#2305=FACE_OUTER_BOUND('',#3353,.T.);
#2306=FACE_OUTER_BOUND('',#3354,.T.);
#2307=FACE_OUTER_BOUND('',#3355,.T.);
#2308=FACE_OUTER_BOUND('',#3357,.T.);
#2309=FACE_OUTER_BOUND('',#3359,.T.);
#2310=FACE_OUTER_BOUND('',#3361,.T.);
#2311=FACE_OUTER_BOUND('',#3363,.T.);
#2312=FACE_OUTER_BOUND('',#3364,.T.);
#2313=FACE_OUTER_BOUND('',#3365,.T.);
#2314=FACE_OUTER_BOUND('',#3369,.T.);
#2315=FACE_OUTER_BOUND('',#3370,.T.);
#2316=FACE_OUTER_BOUND('',#3371,.T.);
#2317=FACE_OUTER_BOUND('',#3375,.T.);
#2318=FACE_OUTER_BOUND('',#3377,.T.);
#2319=FACE_OUTER_BOUND('',#3379,.T.);
#2320=FACE_OUTER_BOUND('',#3380,.T.);
#2321=FACE_OUTER_BOUND('',#3382,.T.);
#2322=FACE_OUTER_BOUND('',#3384,.T.);
#2323=FACE_OUTER_BOUND('',#3385,.T.);
#2324=FACE_OUTER_BOUND('',#3387,.T.);
#2325=FACE_OUTER_BOUND('',#3388,.T.);
#2326=FACE_OUTER_BOUND('',#3389,.T.);
#2327=FACE_OUTER_BOUND('',#3390,.T.);
#2328=FACE_OUTER_BOUND('',#3391,.T.);
#2329=FACE_OUTER_BOUND('',#3392,.T.);
#2330=FACE_OUTER_BOUND('',#3393,.T.);
#2331=FACE_OUTER_BOUND('',#3394,.T.);
#2332=FACE_OUTER_BOUND('',#3395,.T.);
#2333=FACE_OUTER_BOUND('',#3396,.T.);
#2334=FACE_OUTER_BOUND('',#3397,.T.);
#2335=FACE_OUTER_BOUND('',#3398,.T.);
#2336=FACE_OUTER_BOUND('',#3399,.T.);
#2337=FACE_OUTER_BOUND('',#3400,.T.);
#2338=FACE_OUTER_BOUND('',#3401,.T.);
#2339=FACE_OUTER_BOUND('',#3402,.T.);
#2340=FACE_OUTER_BOUND('',#3403,.T.);
#2341=FACE_OUTER_BOUND('',#3404,.T.);
#2342=FACE_OUTER_BOUND('',#3405,.T.);
#2343=FACE_OUTER_BOUND('',#3406,.T.);
#2344=FACE_OUTER_BOUND('',#3407,.T.);
#2345=FACE_OUTER_BOUND('',#3408,.T.);
#2346=FACE_OUTER_BOUND('',#3409,.T.);
#2347=FACE_OUTER_BOUND('',#3410,.T.);
#2348=FACE_OUTER_BOUND('',#3411,.T.);
#2349=FACE_OUTER_BOUND('',#3412,.T.);
#2350=FACE_OUTER_BOUND('',#3413,.T.);
#2351=FACE_OUTER_BOUND('',#3414,.T.);
#2352=FACE_OUTER_BOUND('',#3415,.T.);
#2353=FACE_OUTER_BOUND('',#3416,.T.);
#2354=FACE_OUTER_BOUND('',#3417,.T.);
#2355=FACE_OUTER_BOUND('',#3418,.T.);
#2356=FACE_OUTER_BOUND('',#3419,.T.);
#2357=FACE_OUTER_BOUND('',#3420,.T.);
#2358=FACE_OUTER_BOUND('',#3421,.T.);
#2359=FACE_OUTER_BOUND('',#3422,.T.);
#2360=FACE_OUTER_BOUND('',#3423,.T.);
#2361=FACE_OUTER_BOUND('',#3424,.T.);
#2362=FACE_OUTER_BOUND('',#3425,.T.);
#2363=FACE_OUTER_BOUND('',#3426,.T.);
#2364=FACE_OUTER_BOUND('',#3427,.T.);
#2365=FACE_OUTER_BOUND('',#3428,.T.);
#2366=FACE_OUTER_BOUND('',#3429,.T.);
#2367=FACE_OUTER_BOUND('',#3430,.T.);
#2368=FACE_OUTER_BOUND('',#3431,.T.);
#2369=FACE_OUTER_BOUND('',#3432,.T.);
#2370=FACE_OUTER_BOUND('',#3433,.T.);
#2371=FACE_OUTER_BOUND('',#3434,.T.);
#2372=FACE_OUTER_BOUND('',#3435,.T.);
#2373=FACE_OUTER_BOUND('',#3436,.T.);
#2374=FACE_OUTER_BOUND('',#3437,.T.);
#2375=FACE_OUTER_BOUND('',#3438,.T.);
#2376=FACE_OUTER_BOUND('',#3439,.T.);
#2377=FACE_OUTER_BOUND('',#3440,.T.);
#2378=FACE_OUTER_BOUND('',#3441,.T.);
#2379=FACE_OUTER_BOUND('',#3442,.T.);
#2380=FACE_OUTER_BOUND('',#3443,.T.);
#2381=FACE_OUTER_BOUND('',#3444,.T.);
#2382=FACE_OUTER_BOUND('',#3445,.T.);
#2383=FACE_OUTER_BOUND('',#3446,.T.);
#2384=FACE_OUTER_BOUND('',#3447,.T.);
#2385=FACE_OUTER_BOUND('',#3448,.T.);
#2386=FACE_OUTER_BOUND('',#3449,.T.);
#2387=FACE_OUTER_BOUND('',#3450,.T.);
#2388=FACE_OUTER_BOUND('',#3451,.T.);
#2389=FACE_OUTER_BOUND('',#3452,.T.);
#2390=FACE_OUTER_BOUND('',#3453,.T.);
#2391=FACE_OUTER_BOUND('',#3454,.T.);
#2392=FACE_OUTER_BOUND('',#3455,.T.);
#2393=FACE_OUTER_BOUND('',#3456,.T.);
#2394=FACE_OUTER_BOUND('',#3457,.T.);
#2395=FACE_OUTER_BOUND('',#3458,.T.);
#2396=FACE_OUTER_BOUND('',#3459,.T.);
#2397=FACE_OUTER_BOUND('',#3460,.T.);
#2398=FACE_OUTER_BOUND('',#3461,.T.);
#2399=FACE_OUTER_BOUND('',#3462,.T.);
#2400=FACE_OUTER_BOUND('',#3463,.T.);
#2401=FACE_OUTER_BOUND('',#3464,.T.);
#2402=FACE_OUTER_BOUND('',#3465,.T.);
#2403=FACE_OUTER_BOUND('',#3466,.T.);
#2404=FACE_OUTER_BOUND('',#3467,.T.);
#2405=FACE_OUTER_BOUND('',#3468,.T.);
#2406=FACE_OUTER_BOUND('',#3469,.T.);
#2407=FACE_OUTER_BOUND('',#3470,.T.);
#2408=FACE_OUTER_BOUND('',#3471,.T.);
#2409=FACE_OUTER_BOUND('',#3473,.T.);
#2410=FACE_OUTER_BOUND('',#3474,.T.);
#2411=FACE_OUTER_BOUND('',#3475,.T.);
#2412=FACE_OUTER_BOUND('',#3476,.T.);
#2413=FACE_OUTER_BOUND('',#3477,.T.);
#2414=FACE_OUTER_BOUND('',#3478,.T.);
#2415=FACE_OUTER_BOUND('',#3479,.T.);
#2416=FACE_OUTER_BOUND('',#3480,.T.);
#2417=FACE_OUTER_BOUND('',#3481,.T.);
#2418=FACE_OUTER_BOUND('',#3482,.T.);
#2419=FACE_OUTER_BOUND('',#3483,.T.);
#2420=FACE_OUTER_BOUND('',#3484,.T.);
#2421=FACE_OUTER_BOUND('',#3485,.T.);
#2422=FACE_OUTER_BOUND('',#3486,.T.);
#2423=FACE_OUTER_BOUND('',#3487,.T.);
#2424=FACE_OUTER_BOUND('',#3488,.T.);
#2425=FACE_OUTER_BOUND('',#3489,.T.);
#2426=FACE_OUTER_BOUND('',#3490,.T.);
#2427=FACE_OUTER_BOUND('',#3491,.T.);
#2428=FACE_OUTER_BOUND('',#3492,.T.);
#2429=FACE_OUTER_BOUND('',#3494,.T.);
#2430=FACE_OUTER_BOUND('',#3495,.T.);
#2431=FACE_OUTER_BOUND('',#3496,.T.);
#2432=FACE_OUTER_BOUND('',#3497,.T.);
#2433=EDGE_LOOP('',(#8958,#8959,#8960,#8961));
#2434=EDGE_LOOP('',(#8962));
#2435=EDGE_LOOP('',(#8963,#8964,#8965,#8966));
#2436=EDGE_LOOP('',(#8967));
#2437=EDGE_LOOP('',(#8968,#8969,#8970,#8971));
#2438=EDGE_LOOP('',(#8972));
#2439=EDGE_LOOP('',(#8973,#8974,#8975,#8976));
#2440=EDGE_LOOP('',(#8977));
#2441=EDGE_LOOP('',(#8978,#8979,#8980,#8981));
#2442=EDGE_LOOP('',(#8982));
#2443=EDGE_LOOP('',(#8983,#8984,#8985,#8986));
#2444=EDGE_LOOP('',(#8987));
#2445=EDGE_LOOP('',(#8988,#8989,#8990,#8991));
#2446=EDGE_LOOP('',(#8992));
#2447=EDGE_LOOP('',(#8993,#8994,#8995,#8996));
#2448=EDGE_LOOP('',(#8997));
#2449=EDGE_LOOP('',(#8998,#8999,#9000,#9001));
#2450=EDGE_LOOP('',(#9002));
#2451=EDGE_LOOP('',(#9003,#9004,#9005,#9006));
#2452=EDGE_LOOP('',(#9007));
#2453=EDGE_LOOP('',(#9008,#9009,#9010,#9011));
#2454=EDGE_LOOP('',(#9012,#9013,#9014,#9015));
#2455=EDGE_LOOP('',(#9016,#9017,#9018,#9019));
#2456=EDGE_LOOP('',(#9020,#9021,#9022,#9023));
#2457=EDGE_LOOP('',(#9024,#9025,#9026,#9027));
#2458=EDGE_LOOP('',(#9028,#9029,#9030,#9031));
#2459=EDGE_LOOP('',(#9032,#9033,#9034,#9035));
#2460=EDGE_LOOP('',(#9036,#9037,#9038,#9039));
#2461=EDGE_LOOP('',(#9040,#9041,#9042,#9043));
#2462=EDGE_LOOP('',(#9044,#9045,#9046,#9047));
#2463=EDGE_LOOP('',(#9048,#9049,#9050,#9051));
#2464=EDGE_LOOP('',(#9052,#9053,#9054,#9055));
#2465=EDGE_LOOP('',(#9056,#9057,#9058,#9059));
#2466=EDGE_LOOP('',(#9060,#9061,#9062,#9063,#9064,#9065,#9066,#9067));
#2467=EDGE_LOOP('',(#9068,#9069,#9070,#9071));
#2468=EDGE_LOOP('',(#9072,#9073,#9074,#9075));
#2469=EDGE_LOOP('',(#9076,#9077,#9078,#9079));
#2470=EDGE_LOOP('',(#9080,#9081,#9082,#9083,#9084,#9085,#9086,#9087));
#2471=EDGE_LOOP('',(#9088,#9089,#9090,#9091));
#2472=EDGE_LOOP('',(#9092,#9093,#9094,#9095));
#2473=EDGE_LOOP('',(#9096,#9097,#9098,#9099));
#2474=EDGE_LOOP('',(#9100,#9101,#9102,#9103));
#2475=EDGE_LOOP('',(#9104,#9105));
#2476=EDGE_LOOP('',(#9106,#9107,#9108,#9109));
#2477=EDGE_LOOP('',(#9110));
#2478=EDGE_LOOP('',(#9111,#9112,#9113,#9114));
#2479=EDGE_LOOP('',(#9115));
#2480=EDGE_LOOP('',(#9116,#9117,#9118,#9119));
#2481=EDGE_LOOP('',(#9120,#9121));
#2482=EDGE_LOOP('',(#9122,#9123,#9124,#9125));
#2483=EDGE_LOOP('',(#9126,#9127,#9128,#9129));
#2484=EDGE_LOOP('',(#9130,#9131,#9132,#9133));
#2485=EDGE_LOOP('',(#9134,#9135,#9136,#9137));
#2486=EDGE_LOOP('',(#9138,#9139,#9140,#9141));
#2487=EDGE_LOOP('',(#9142));
#2488=EDGE_LOOP('',(#9143));
#2489=EDGE_LOOP('',(#9144));
#2490=EDGE_LOOP('',(#9145));
#2491=EDGE_LOOP('',(#9146));
#2492=EDGE_LOOP('',(#9147));
#2493=EDGE_LOOP('',(#9148,#9149,#9150,#9151,#9152,#9153));
#2494=EDGE_LOOP('',(#9154,#9155,#9156,#9157,#9158,#9159));
#2495=EDGE_LOOP('',(#9160,#9161,#9162,#9163));
#2496=EDGE_LOOP('',(#9164,#9165,#9166,#9167));
#2497=EDGE_LOOP('',(#9168));
#2498=EDGE_LOOP('',(#9169));
#2499=EDGE_LOOP('',(#9170));
#2500=EDGE_LOOP('',(#9171));
#2501=EDGE_LOOP('',(#9172));
#2502=EDGE_LOOP('',(#9173));
#2503=EDGE_LOOP('',(#9174,#9175,#9176,#9177));
#2504=EDGE_LOOP('',(#9178,#9179,#9180,#9181));
#2505=EDGE_LOOP('',(#9182,#9183,#9184,#9185));
#2506=EDGE_LOOP('',(#9186,#9187,#9188,#9189));
#2507=EDGE_LOOP('',(#9190,#9191,#9192,#9193));
#2508=EDGE_LOOP('',(#9194,#9195,#9196,#9197));
#2509=EDGE_LOOP('',(#9198,#9199,#9200,#9201));
#2510=EDGE_LOOP('',(#9202,#9203,#9204,#9205));
#2511=EDGE_LOOP('',(#9206,#9207,#9208,#9209));
#2512=EDGE_LOOP('',(#9210,#9211,#9212,#9213));
#2513=EDGE_LOOP('',(#9214,#9215,#9216,#9217));
#2514=EDGE_LOOP('',(#9218,#9219,#9220,#9221));
#2515=EDGE_LOOP('',(#9222,#9223,#9224,#9225));
#2516=EDGE_LOOP('',(#9226,#9227,#9228,#9229));
#2517=EDGE_LOOP('',(#9230,#9231,#9232,#9233));
#2518=EDGE_LOOP('',(#9234,#9235,#9236,#9237));
#2519=EDGE_LOOP('',(#9238,#9239,#9240,#9241));
#2520=EDGE_LOOP('',(#9242,#9243,#9244,#9245));
#2521=EDGE_LOOP('',(#9246,#9247,#9248,#9249));
#2522=EDGE_LOOP('',(#9250,#9251,#9252,#9253));
#2523=EDGE_LOOP('',(#9254,#9255,#9256,#9257));
#2524=EDGE_LOOP('',(#9258,#9259,#9260,#9261));
#2525=EDGE_LOOP('',(#9262));
#2526=EDGE_LOOP('',(#9263));
#2527=EDGE_LOOP('',(#9264,#9265,#9266,#9267));
#2528=EDGE_LOOP('',(#9268));
#2529=EDGE_LOOP('',(#9269));
#2530=EDGE_LOOP('',(#9270,#9271,#9272,#9273));
#2531=EDGE_LOOP('',(#9274,#9275,#9276,#9277));
#2532=EDGE_LOOP('',(#9278,#9279,#9280,#9281,#9282,#9283,#9284,#9285));
#2533=EDGE_LOOP('',(#9286));
#2534=EDGE_LOOP('',(#9287));
#2535=EDGE_LOOP('',(#9288));
#2536=EDGE_LOOP('',(#9289));
#2537=EDGE_LOOP('',(#9290));
#2538=EDGE_LOOP('',(#9291,#9292,#9293,#9294));
#2539=EDGE_LOOP('',(#9295,#9296,#9297,#9298,#9299,#9300,#9301,#9302));
#2540=EDGE_LOOP('',(#9303));
#2541=EDGE_LOOP('',(#9304));
#2542=EDGE_LOOP('',(#9305));
#2543=EDGE_LOOP('',(#9306));
#2544=EDGE_LOOP('',(#9307));
#2545=EDGE_LOOP('',(#9308,#9309,#9310,#9311));
#2546=EDGE_LOOP('',(#9312,#9313,#9314,#9315));
#2547=EDGE_LOOP('',(#9316,#9317,#9318,#9319));
#2548=EDGE_LOOP('',(#9320));
#2549=EDGE_LOOP('',(#9321));
#2550=EDGE_LOOP('',(#9322));
#2551=EDGE_LOOP('',(#9323));
#2552=EDGE_LOOP('',(#9324,#9325,#9326,#9327));
#2553=EDGE_LOOP('',(#9328,#9329,#9330,#9331));
#2554=EDGE_LOOP('',(#9332));
#2555=EDGE_LOOP('',(#9333));
#2556=EDGE_LOOP('',(#9334));
#2557=EDGE_LOOP('',(#9335));
#2558=EDGE_LOOP('',(#9336,#9337,#9338,#9339));
#2559=EDGE_LOOP('',(#9340,#9341,#9342,#9343));
#2560=EDGE_LOOP('',(#9344,#9345,#9346,#9347));
#2561=EDGE_LOOP('',(#9348,#9349,#9350,#9351));
#2562=EDGE_LOOP('',(#9352,#9353,#9354,#9355,#9356,#9357,#9358,#9359));
#2563=EDGE_LOOP('',(#9360));
#2564=EDGE_LOOP('',(#9361,#9362,#9363,#9364));
#2565=EDGE_LOOP('',(#9365,#9366,#9367,#9368));
#2566=EDGE_LOOP('',(#9369,#9370,#9371,#9372));
#2567=EDGE_LOOP('',(#9373,#9374,#9375,#9376));
#2568=EDGE_LOOP('',(#9377,#9378,#9379,#9380));
#2569=EDGE_LOOP('',(#9381));
#2570=EDGE_LOOP('',(#9382));
#2571=EDGE_LOOP('',(#9383,#9384,#9385,#9386));
#2572=EDGE_LOOP('',(#9387,#9388,#9389,#9390,#9391,#9392,#9393,#9394));
#2573=EDGE_LOOP('',(#9395));
#2574=EDGE_LOOP('',(#9396,#9397,#9398,#9399));
#2575=EDGE_LOOP('',(#9400,#9401,#9402,#9403));
#2576=EDGE_LOOP('',(#9404,#9405,#9406,#9407));
#2577=EDGE_LOOP('',(#9408,#9409,#9410,#9411));
#2578=EDGE_LOOP('',(#9412,#9413,#9414,#9415,#9416,#9417,#9418,#9419));
#2579=EDGE_LOOP('',(#9420));
#2580=EDGE_LOOP('',(#9421,#9422,#9423,#9424));
#2581=EDGE_LOOP('',(#9425,#9426,#9427,#9428));
#2582=EDGE_LOOP('',(#9429,#9430,#9431,#9432));
#2583=EDGE_LOOP('',(#9433,#9434,#9435,#9436));
#2584=EDGE_LOOP('',(#9437,#9438,#9439,#9440));
#2585=EDGE_LOOP('',(#9441));
#2586=EDGE_LOOP('',(#9442));
#2587=EDGE_LOOP('',(#9443,#9444,#9445,#9446));
#2588=EDGE_LOOP('',(#9447,#9448,#9449,#9450,#9451,#9452,#9453,#9454));
#2589=EDGE_LOOP('',(#9455));
#2590=EDGE_LOOP('',(#9456,#9457,#9458,#9459));
#2591=EDGE_LOOP('',(#9460,#9461,#9462,#9463));
#2592=EDGE_LOOP('',(#9464,#9465,#9466,#9467,#9468,#9469));
#2593=EDGE_LOOP('',(#9470));
#2594=EDGE_LOOP('',(#9471));
#2595=EDGE_LOOP('',(#9472));
#2596=EDGE_LOOP('',(#9473));
#2597=EDGE_LOOP('',(#9474));
#2598=EDGE_LOOP('',(#9475,#9476,#9477,#9478));
#2599=EDGE_LOOP('',(#9479,#9480,#9481,#9482,#9483,#9484,#9485,#9486));
#2600=EDGE_LOOP('',(#9487,#9488,#9489,#9490,#9491,#9492,#9493,#9494));
#2601=EDGE_LOOP('',(#9495,#9496,#9497));
#2602=EDGE_LOOP('',(#9498,#9499,#9500));
#2603=EDGE_LOOP('',(#9501,#9502,#9503,#9504));
#2604=EDGE_LOOP('',(#9505,#9506,#9507,#9508));
#2605=EDGE_LOOP('',(#9509,#9510,#9511,#9512));
#2606=EDGE_LOOP('',(#9513,#9514,#9515,#9516));
#2607=EDGE_LOOP('',(#9517,#9518,#9519,#9520));
#2608=EDGE_LOOP('',(#9521,#9522,#9523,#9524));
#2609=EDGE_LOOP('',(#9525,#9526,#9527,#9528));
#2610=EDGE_LOOP('',(#9529,#9530,#9531,#9532));
#2611=EDGE_LOOP('',(#9533,#9534,#9535,#9536));
#2612=EDGE_LOOP('',(#9537,#9538,#9539,#9540));
#2613=EDGE_LOOP('',(#9541));
#2614=EDGE_LOOP('',(#9542));
#2615=EDGE_LOOP('',(#9543,#9544,#9545,#9546));
#2616=EDGE_LOOP('',(#9547));
#2617=EDGE_LOOP('',(#9548));
#2618=EDGE_LOOP('',(#9549,#9550,#9551,#9552));
#2619=EDGE_LOOP('',(#9553,#9554,#9555,#9556));
#2620=EDGE_LOOP('',(#9557,#9558,#9559,#9560,#9561,#9562,#9563,#9564));
#2621=EDGE_LOOP('',(#9565));
#2622=EDGE_LOOP('',(#9566));
#2623=EDGE_LOOP('',(#9567));
#2624=EDGE_LOOP('',(#9568));
#2625=EDGE_LOOP('',(#9569));
#2626=EDGE_LOOP('',(#9570,#9571,#9572,#9573,#9574,#9575,#9576,#9577));
#2627=EDGE_LOOP('',(#9578,#9579,#9580,#9581,#9582,#9583,#9584,#9585));
#2628=EDGE_LOOP('',(#9586,#9587,#9588,#9589));
#2629=EDGE_LOOP('',(#9590));
#2630=EDGE_LOOP('',(#9591));
#2631=EDGE_LOOP('',(#9592));
#2632=EDGE_LOOP('',(#9593));
#2633=EDGE_LOOP('',(#9594,#9595,#9596,#9597));
#2634=EDGE_LOOP('',(#9598,#9599,#9600,#9601));
#2635=EDGE_LOOP('',(#9602));
#2636=EDGE_LOOP('',(#9603));
#2637=EDGE_LOOP('',(#9604));
#2638=EDGE_LOOP('',(#9605));
#2639=EDGE_LOOP('',(#9606,#9607,#9608,#9609));
#2640=EDGE_LOOP('',(#9610,#9611,#9612,#9613));
#2641=EDGE_LOOP('',(#9614));
#2642=EDGE_LOOP('',(#9615));
#2643=EDGE_LOOP('',(#9616));
#2644=EDGE_LOOP('',(#9617));
#2645=EDGE_LOOP('',(#9618,#9619,#9620,#9621));
#2646=EDGE_LOOP('',(#9622,#9623,#9624,#9625));
#2647=EDGE_LOOP('',(#9626));
#2648=EDGE_LOOP('',(#9627));
#2649=EDGE_LOOP('',(#9628));
#2650=EDGE_LOOP('',(#9629));
#2651=EDGE_LOOP('',(#9630,#9631,#9632,#9633));
#2652=EDGE_LOOP('',(#9634,#9635,#9636,#9637));
#2653=EDGE_LOOP('',(#9638));
#2654=EDGE_LOOP('',(#9639));
#2655=EDGE_LOOP('',(#9640));
#2656=EDGE_LOOP('',(#9641));
#2657=EDGE_LOOP('',(#9642,#9643,#9644,#9645));
#2658=EDGE_LOOP('',(#9646,#9647,#9648,#9649));
#2659=EDGE_LOOP('',(#9650));
#2660=EDGE_LOOP('',(#9651));
#2661=EDGE_LOOP('',(#9652));
#2662=EDGE_LOOP('',(#9653));
#2663=EDGE_LOOP('',(#9654,#9655,#9656,#9657));
#2664=EDGE_LOOP('',(#9658,#9659,#9660,#9661));
#2665=EDGE_LOOP('',(#9662,#9663,#9664,#9665));
#2666=EDGE_LOOP('',(#9666,#9667,#9668,#9669));
#2667=EDGE_LOOP('',(#9670,#9671,#9672,#9673,#9674,#9675,#9676,#9677));
#2668=EDGE_LOOP('',(#9678));
#2669=EDGE_LOOP('',(#9679,#9680,#9681,#9682));
#2670=EDGE_LOOP('',(#9683,#9684,#9685,#9686));
#2671=EDGE_LOOP('',(#9687,#9688,#9689,#9690));
#2672=EDGE_LOOP('',(#9691,#9692,#9693,#9694));
#2673=EDGE_LOOP('',(#9695,#9696,#9697,#9698));
#2674=EDGE_LOOP('',(#9699));
#2675=EDGE_LOOP('',(#9700));
#2676=EDGE_LOOP('',(#9701,#9702,#9703,#9704));
#2677=EDGE_LOOP('',(#9705,#9706,#9707,#9708,#9709,#9710,#9711,#9712));
#2678=EDGE_LOOP('',(#9713));
#2679=EDGE_LOOP('',(#9714,#9715,#9716,#9717));
#2680=EDGE_LOOP('',(#9718,#9719,#9720,#9721));
#2681=EDGE_LOOP('',(#9722,#9723,#9724,#9725));
#2682=EDGE_LOOP('',(#9726,#9727,#9728,#9729));
#2683=EDGE_LOOP('',(#9730,#9731,#9732,#9733));
#2684=EDGE_LOOP('',(#9734,#9735,#9736,#9737));
#2685=EDGE_LOOP('',(#9738,#9739,#9740,#9741));
#2686=EDGE_LOOP('',(#9742,#9743,#9744,#9745));
#2687=EDGE_LOOP('',(#9746,#9747,#9748,#9749));
#2688=EDGE_LOOP('',(#9750,#9751,#9752,#9753));
#2689=EDGE_LOOP('',(#9754,#9755,#9756,#9757));
#2690=EDGE_LOOP('',(#9758,#9759,#9760,#9761,#9762,#9763,#9764,#9765));
#2691=EDGE_LOOP('',(#9766,#9767,#9768,#9769,#9770,#9771,#9772,#9773));
#2692=EDGE_LOOP('',(#9774));
#2693=EDGE_LOOP('',(#9775,#9776,#9777,#9778,#9779,#9780,#9781,#9782));
#2694=EDGE_LOOP('',(#9783));
#2695=EDGE_LOOP('',(#9784,#9785,#9786,#9787,#9788,#9789,#9790,#9791));
#2696=EDGE_LOOP('',(#9792,#9793,#9794,#9795,#9796,#9797,#9798,#9799));
#2697=EDGE_LOOP('',(#9800,#9801,#9802,#9803));
#2698=EDGE_LOOP('',(#9804,#9805,#9806,#9807,#9808,#9809,#9810,#9811));
#2699=EDGE_LOOP('',(#9812,#9813,#9814,#9815));
#2700=EDGE_LOOP('',(#9816,#9817,#9818,#9819));
#2701=EDGE_LOOP('',(#9820,#9821,#9822,#9823));
#2702=EDGE_LOOP('',(#9824,#9825,#9826,#9827));
#2703=EDGE_LOOP('',(#9828,#9829,#9830,#9831));
#2704=EDGE_LOOP('',(#9832,#9833,#9834,#9835));
#2705=EDGE_LOOP('',(#9836,#9837,#9838,#9839));
#2706=EDGE_LOOP('',(#9840,#9841,#9842,#9843));
#2707=EDGE_LOOP('',(#9844,#9845,#9846,#9847));
#2708=EDGE_LOOP('',(#9848,#9849,#9850,#9851));
#2709=EDGE_LOOP('',(#9852,#9853,#9854,#9855));
#2710=EDGE_LOOP('',(#9856,#9857,#9858,#9859));
#2711=EDGE_LOOP('',(#9860,#9861,#9862,#9863));
#2712=EDGE_LOOP('',(#9864,#9865,#9866,#9867));
#2713=EDGE_LOOP('',(#9868));
#2714=EDGE_LOOP('',(#9869));
#2715=EDGE_LOOP('',(#9870,#9871,#9872,#9873));
#2716=EDGE_LOOP('',(#9874,#9875,#9876,#9877));
#2717=EDGE_LOOP('',(#9878));
#2718=EDGE_LOOP('',(#9879));
#2719=EDGE_LOOP('',(#9880,#9881,#9882,#9883));
#2720=EDGE_LOOP('',(#9884,#9885,#9886,#9887));
#2721=EDGE_LOOP('',(#9888));
#2722=EDGE_LOOP('',(#9889));
#2723=EDGE_LOOP('',(#9890,#9891,#9892,#9893));
#2724=EDGE_LOOP('',(#9894,#9895,#9896,#9897));
#2725=EDGE_LOOP('',(#9898));
#2726=EDGE_LOOP('',(#9899));
#2727=EDGE_LOOP('',(#9900,#9901,#9902,#9903));
#2728=EDGE_LOOP('',(#9904,#9905,#9906,#9907));
#2729=EDGE_LOOP('',(#9908));
#2730=EDGE_LOOP('',(#9909,#9910,#9911,#9912));
#2731=EDGE_LOOP('',(#9913));
#2732=EDGE_LOOP('',(#9914,#9915,#9916,#9917));
#2733=EDGE_LOOP('',(#9918,#9919,#9920,#9921));
#2734=EDGE_LOOP('',(#9922,#9923,#9924,#9925));
#2735=EDGE_LOOP('',(#9926,#9927,#9928,#9929));
#2736=EDGE_LOOP('',(#9930,#9931,#9932,#9933));
#2737=EDGE_LOOP('',(#9934));
#2738=EDGE_LOOP('',(#9935));
#2739=EDGE_LOOP('',(#9936));
#2740=EDGE_LOOP('',(#9937));
#2741=EDGE_LOOP('',(#9938));
#2742=EDGE_LOOP('',(#9939));
#2743=EDGE_LOOP('',(#9940,#9941,#9942,#9943));
#2744=EDGE_LOOP('',(#9944));
#2745=EDGE_LOOP('',(#9945));
#2746=EDGE_LOOP('',(#9946));
#2747=EDGE_LOOP('',(#9947));
#2748=EDGE_LOOP('',(#9948,#9949,#9950,#9951));
#2749=EDGE_LOOP('',(#9952,#9953,#9954,#9955));
#2750=EDGE_LOOP('',(#9956));
#2751=EDGE_LOOP('',(#9957));
#2752=EDGE_LOOP('',(#9958));
#2753=EDGE_LOOP('',(#9959));
#2754=EDGE_LOOP('',(#9960,#9961,#9962,#9963));
#2755=EDGE_LOOP('',(#9964,#9965,#9966,#9967));
#2756=EDGE_LOOP('',(#9968));
#2757=EDGE_LOOP('',(#9969));
#2758=EDGE_LOOP('',(#9970));
#2759=EDGE_LOOP('',(#9971));
#2760=EDGE_LOOP('',(#9972,#9973,#9974,#9975));
#2761=EDGE_LOOP('',(#9976));
#2762=EDGE_LOOP('',(#9977));
#2763=EDGE_LOOP('',(#9978,#9979,#9980,#9981));
#2764=EDGE_LOOP('',(#9982,#9983,#9984,#9985));
#2765=EDGE_LOOP('',(#9986));
#2766=EDGE_LOOP('',(#9987));
#2767=EDGE_LOOP('',(#9988,#9989,#9990,#9991));
#2768=EDGE_LOOP('',(#9992,#9993,#9994,#9995));
#2769=EDGE_LOOP('',(#9996));
#2770=EDGE_LOOP('',(#9997));
#2771=EDGE_LOOP('',(#9998,#9999,#10000,#10001));
#2772=EDGE_LOOP('',(#10002,#10003,#10004,#10005));
#2773=EDGE_LOOP('',(#10006));
#2774=EDGE_LOOP('',(#10007));
#2775=EDGE_LOOP('',(#10008,#10009,#10010,#10011));
#2776=EDGE_LOOP('',(#10012,#10013,#10014,#10015));
#2777=EDGE_LOOP('',(#10016));
#2778=EDGE_LOOP('',(#10017,#10018,#10019,#10020));
#2779=EDGE_LOOP('',(#10021));
#2780=EDGE_LOOP('',(#10022,#10023,#10024,#10025));
#2781=EDGE_LOOP('',(#10026,#10027,#10028,#10029));
#2782=EDGE_LOOP('',(#10030,#10031,#10032,#10033));
#2783=EDGE_LOOP('',(#10034,#10035,#10036,#10037));
#2784=EDGE_LOOP('',(#10038,#10039,#10040,#10041));
#2785=EDGE_LOOP('',(#10042));
#2786=EDGE_LOOP('',(#10043));
#2787=EDGE_LOOP('',(#10044));
#2788=EDGE_LOOP('',(#10045));
#2789=EDGE_LOOP('',(#10046));
#2790=EDGE_LOOP('',(#10047));
#2791=EDGE_LOOP('',(#10048,#10049,#10050,#10051));
#2792=EDGE_LOOP('',(#10052));
#2793=EDGE_LOOP('',(#10053));
#2794=EDGE_LOOP('',(#10054));
#2795=EDGE_LOOP('',(#10055));
#2796=EDGE_LOOP('',(#10056,#10057,#10058,#10059));
#2797=EDGE_LOOP('',(#10060,#10061,#10062,#10063));
#2798=EDGE_LOOP('',(#10064));
#2799=EDGE_LOOP('',(#10065));
#2800=EDGE_LOOP('',(#10066));
#2801=EDGE_LOOP('',(#10067));
#2802=EDGE_LOOP('',(#10068,#10069,#10070,#10071));
#2803=EDGE_LOOP('',(#10072,#10073,#10074,#10075));
#2804=EDGE_LOOP('',(#10076));
#2805=EDGE_LOOP('',(#10077));
#2806=EDGE_LOOP('',(#10078));
#2807=EDGE_LOOP('',(#10079));
#2808=EDGE_LOOP('',(#10080,#10081,#10082,#10083));
#2809=EDGE_LOOP('',(#10084));
#2810=EDGE_LOOP('',(#10085));
#2811=EDGE_LOOP('',(#10086,#10087,#10088,#10089));
#2812=EDGE_LOOP('',(#10090,#10091,#10092,#10093));
#2813=EDGE_LOOP('',(#10094));
#2814=EDGE_LOOP('',(#10095));
#2815=EDGE_LOOP('',(#10096,#10097,#10098,#10099));
#2816=EDGE_LOOP('',(#10100,#10101,#10102,#10103));
#2817=EDGE_LOOP('',(#10104,#10105,#10106,#10107));
#2818=EDGE_LOOP('',(#10108,#10109,#10110,#10111));
#2819=EDGE_LOOP('',(#10112,#10113,#10114,#10115));
#2820=EDGE_LOOP('',(#10116,#10117,#10118,#10119));
#2821=EDGE_LOOP('',(#10120));
#2822=EDGE_LOOP('',(#10121));
#2823=EDGE_LOOP('',(#10122,#10123,#10124,#10125));
#2824=EDGE_LOOP('',(#10126));
#2825=EDGE_LOOP('',(#10127));
#2826=EDGE_LOOP('',(#10128,#10129,#10130,#10131));
#2827=EDGE_LOOP('',(#10132,#10133,#10134,#10135));
#2828=EDGE_LOOP('',(#10136,#10137,#10138,#10139));
#2829=EDGE_LOOP('',(#10140,#10141,#10142,#10143));
#2830=EDGE_LOOP('',(#10144,#10145,#10146,#10147));
#2831=EDGE_LOOP('',(#10148,#10149,#10150,#10151));
#2832=EDGE_LOOP('',(#10152,#10153,#10154,#10155));
#2833=EDGE_LOOP('',(#10156,#10157,#10158,#10159));
#2834=EDGE_LOOP('',(#10160,#10161,#10162,#10163));
#2835=EDGE_LOOP('',(#10164));
#2836=EDGE_LOOP('',(#10165));
#2837=EDGE_LOOP('',(#10166,#10167,#10168,#10169));
#2838=EDGE_LOOP('',(#10170,#10171,#10172,#10173));
#2839=EDGE_LOOP('',(#10174));
#2840=EDGE_LOOP('',(#10175));
#2841=EDGE_LOOP('',(#10176,#10177,#10178,#10179));
#2842=EDGE_LOOP('',(#10180,#10181,#10182,#10183));
#2843=EDGE_LOOP('',(#10184,#10185,#10186,#10187));
#2844=EDGE_LOOP('',(#10188,#10189,#10190,#10191));
#2845=EDGE_LOOP('',(#10192,#10193,#10194,#10195));
#2846=EDGE_LOOP('',(#10196,#10197,#10198,#10199));
#2847=EDGE_LOOP('',(#10200));
#2848=EDGE_LOOP('',(#10201));
#2849=EDGE_LOOP('',(#10202,#10203,#10204,#10205));
#2850=EDGE_LOOP('',(#10206,#10207,#10208,#10209));
#2851=EDGE_LOOP('',(#10210));
#2852=EDGE_LOOP('',(#10211));
#2853=EDGE_LOOP('',(#10212,#10213,#10214,#10215));
#2854=EDGE_LOOP('',(#10216,#10217,#10218,#10219));
#2855=EDGE_LOOP('',(#10220,#10221,#10222,#10223));
#2856=EDGE_LOOP('',(#10224,#10225,#10226,#10227));
#2857=EDGE_LOOP('',(#10228,#10229,#10230,#10231));
#2858=EDGE_LOOP('',(#10232,#10233,#10234,#10235));
#2859=EDGE_LOOP('',(#10236,#10237,#10238,#10239));
#2860=EDGE_LOOP('',(#10240,#10241,#10242,#10243));
#2861=EDGE_LOOP('',(#10244,#10245,#10246,#10247));
#2862=EDGE_LOOP('',(#10248,#10249,#10250,#10251));
#2863=EDGE_LOOP('',(#10252,#10253,#10254,#10255));
#2864=EDGE_LOOP('',(#10256,#10257,#10258,#10259));
#2865=EDGE_LOOP('',(#10260));
#2866=EDGE_LOOP('',(#10261));
#2867=EDGE_LOOP('',(#10262));
#2868=EDGE_LOOP('',(#10263));
#2869=EDGE_LOOP('',(#10264,#10265,#10266,#10267));
#2870=EDGE_LOOP('',(#10268));
#2871=EDGE_LOOP('',(#10269));
#2872=EDGE_LOOP('',(#10270));
#2873=EDGE_LOOP('',(#10271));
#2874=EDGE_LOOP('',(#10272,#10273,#10274,#10275,#10276,#10277));
#2875=EDGE_LOOP('',(#10278,#10279,#10280,#10281,#10282));
#2876=EDGE_LOOP('',(#10283,#10284,#10285,#10286));
#2877=EDGE_LOOP('',(#10287,#10288,#10289,#10290));
#2878=EDGE_LOOP('',(#10291));
#2879=EDGE_LOOP('',(#10292));
#2880=EDGE_LOOP('',(#10293,#10294,#10295,#10296,#10297));
#2881=EDGE_LOOP('',(#10298));
#2882=EDGE_LOOP('',(#10299));
#2883=EDGE_LOOP('',(#10300,#10301,#10302,#10303));
#2884=EDGE_LOOP('',(#10304,#10305,#10306,#10307,#10308,#10309));
#2885=EDGE_LOOP('',(#10310,#10311,#10312,#10313,#10314));
#2886=EDGE_LOOP('',(#10315));
#2887=EDGE_LOOP('',(#10316));
#2888=EDGE_LOOP('',(#10317,#10318,#10319,#10320));
#2889=EDGE_LOOP('',(#10321,#10322,#10323,#10324));
#2890=EDGE_LOOP('',(#10325,#10326,#10327,#10328));
#2891=EDGE_LOOP('',(#10329));
#2892=EDGE_LOOP('',(#10330));
#2893=EDGE_LOOP('',(#10331,#10332,#10333,#10334,#10335));
#2894=EDGE_LOOP('',(#10336,#10337));
#2895=EDGE_LOOP('',(#10338,#10339));
#2896=EDGE_LOOP('',(#10340,#10341));
#2897=EDGE_LOOP('',(#10342,#10343));
#2898=EDGE_LOOP('',(#10344,#10345));
#2899=EDGE_LOOP('',(#10346,#10347));
#2900=EDGE_LOOP('',(#10348,#10349));
#2901=EDGE_LOOP('',(#10350,#10351));
#2902=EDGE_LOOP('',(#10352,#10353,#10354,#10355));
#2903=EDGE_LOOP('',(#10356,#10357,#10358,#10359,#10360,#10361,#10362,#10363,
#10364,#10365,#10366,#10367,#10368,#10369,#10370,#10371,#10372,#10373,#10374,
#10375));
#2904=EDGE_LOOP('',(#10376,#10377,#10378,#10379));
#2905=EDGE_LOOP('',(#10380,#10381,#10382,#10383));
#2906=EDGE_LOOP('',(#10384,#10385,#10386,#10387));
#2907=EDGE_LOOP('',(#10388,#10389,#10390,#10391));
#2908=EDGE_LOOP('',(#10392,#10393,#10394,#10395));
#2909=EDGE_LOOP('',(#10396,#10397,#10398,#10399,#10400,#10401));
#2910=EDGE_LOOP('',(#10402,#10403,#10404,#10405));
#2911=EDGE_LOOP('',(#10406,#10407,#10408,#10409));
#2912=EDGE_LOOP('',(#10410,#10411,#10412,#10413));
#2913=EDGE_LOOP('',(#10414,#10415,#10416,#10417));
#2914=EDGE_LOOP('',(#10418,#10419,#10420,#10421));
#2915=EDGE_LOOP('',(#10422,#10423,#10424,#10425));
#2916=EDGE_LOOP('',(#10426,#10427,#10428,#10429,#10430,#10431,#10432,#10433,
#10434,#10435,#10436,#10437,#10438,#10439,#10440,#10441,#10442,#10443,#10444,
#10445));
#2917=EDGE_LOOP('',(#10446,#10447,#10448,#10449));
#2918=EDGE_LOOP('',(#10450,#10451,#10452,#10453));
#2919=EDGE_LOOP('',(#10454));
#2920=EDGE_LOOP('',(#10455));
#2921=EDGE_LOOP('',(#10456,#10457,#10458,#10459));
#2922=EDGE_LOOP('',(#10460));
#2923=EDGE_LOOP('',(#10461));
#2924=EDGE_LOOP('',(#10462,#10463,#10464,#10465));
#2925=EDGE_LOOP('',(#10466));
#2926=EDGE_LOOP('',(#10467));
#2927=EDGE_LOOP('',(#10468,#10469,#10470,#10471));
#2928=EDGE_LOOP('',(#10472));
#2929=EDGE_LOOP('',(#10473));
#2930=EDGE_LOOP('',(#10474,#10475,#10476,#10477));
#2931=EDGE_LOOP('',(#10478));
#2932=EDGE_LOOP('',(#10479));
#2933=EDGE_LOOP('',(#10480,#10481,#10482,#10483));
#2934=EDGE_LOOP('',(#10484,#10485,#10486,#10487));
#2935=EDGE_LOOP('',(#10488,#10489,#10490,#10491));
#2936=EDGE_LOOP('',(#10492,#10493,#10494,#10495));
#2937=EDGE_LOOP('',(#10496,#10497,#10498,#10499));
#2938=EDGE_LOOP('',(#10500,#10501,#10502,#10503));
#2939=EDGE_LOOP('',(#10504,#10505,#10506,#10507));
#2940=EDGE_LOOP('',(#10508,#10509,#10510,#10511,#10512,#10513));
#2941=EDGE_LOOP('',(#10514,#10515,#10516,#10517,#10518,#10519));
#2942=EDGE_LOOP('',(#10520));
#2943=EDGE_LOOP('',(#10521));
#2944=EDGE_LOOP('',(#10522,#10523,#10524,#10525));
#2945=EDGE_LOOP('',(#10526));
#2946=EDGE_LOOP('',(#10527));
#2947=EDGE_LOOP('',(#10528,#10529,#10530,#10531));
#2948=EDGE_LOOP('',(#10532,#10533,#10534,#10535));
#2949=EDGE_LOOP('',(#10536,#10537,#10538,#10539));
#2950=EDGE_LOOP('',(#10540));
#2951=EDGE_LOOP('',(#10541));
#2952=EDGE_LOOP('',(#10542,#10543,#10544,#10545));
#2953=EDGE_LOOP('',(#10546,#10547,#10548,#10549));
#2954=EDGE_LOOP('',(#10550,#10551,#10552,#10553));
#2955=EDGE_LOOP('',(#10554,#10555,#10556,#10557,#10558,#10559));
#2956=EDGE_LOOP('',(#10560,#10561,#10562,#10563,#10564));
#2957=EDGE_LOOP('',(#10565,#10566,#10567,#10568));
#2958=EDGE_LOOP('',(#10569,#10570,#10571,#10572));
#2959=EDGE_LOOP('',(#10573));
#2960=EDGE_LOOP('',(#10574));
#2961=EDGE_LOOP('',(#10575,#10576,#10577,#10578,#10579));
#2962=EDGE_LOOP('',(#10580));
#2963=EDGE_LOOP('',(#10581));
#2964=EDGE_LOOP('',(#10582,#10583,#10584,#10585));
#2965=EDGE_LOOP('',(#10586,#10587,#10588,#10589,#10590,#10591));
#2966=EDGE_LOOP('',(#10592,#10593,#10594,#10595,#10596));
#2967=EDGE_LOOP('',(#10597));
#2968=EDGE_LOOP('',(#10598));
#2969=EDGE_LOOP('',(#10599,#10600,#10601,#10602));
#2970=EDGE_LOOP('',(#10603,#10604,#10605,#10606));
#2971=EDGE_LOOP('',(#10607,#10608,#10609,#10610));
#2972=EDGE_LOOP('',(#10611));
#2973=EDGE_LOOP('',(#10612));
#2974=EDGE_LOOP('',(#10613,#10614,#10615,#10616,#10617));
#2975=EDGE_LOOP('',(#10618,#10619));
#2976=EDGE_LOOP('',(#10620,#10621));
#2977=EDGE_LOOP('',(#10622,#10623));
#2978=EDGE_LOOP('',(#10624,#10625));
#2979=EDGE_LOOP('',(#10626,#10627));
#2980=EDGE_LOOP('',(#10628,#10629));
#2981=EDGE_LOOP('',(#10630,#10631));
#2982=EDGE_LOOP('',(#10632,#10633,#10634,#10635));
#2983=EDGE_LOOP('',(#10636,#10637,#10638,#10639,#10640,#10641,#10642,#10643,
#10644,#10645,#10646,#10647,#10648,#10649,#10650,#10651,#10652,#10653));
#2984=EDGE_LOOP('',(#10654,#10655,#10656,#10657));
#2985=EDGE_LOOP('',(#10658,#10659,#10660,#10661));
#2986=EDGE_LOOP('',(#10662,#10663,#10664,#10665));
#2987=EDGE_LOOP('',(#10666,#10667,#10668,#10669));
#2988=EDGE_LOOP('',(#10670,#10671,#10672,#10673,#10674,#10675));
#2989=EDGE_LOOP('',(#10676,#10677,#10678,#10679));
#2990=EDGE_LOOP('',(#10680,#10681,#10682,#10683));
#2991=EDGE_LOOP('',(#10684,#10685,#10686,#10687));
#2992=EDGE_LOOP('',(#10688,#10689,#10690,#10691));
#2993=EDGE_LOOP('',(#10692,#10693,#10694,#10695));
#2994=EDGE_LOOP('',(#10696,#10697,#10698,#10699,#10700,#10701,#10702,#10703,
#10704,#10705,#10706,#10707,#10708,#10709,#10710,#10711,#10712,#10713));
#2995=EDGE_LOOP('',(#10714,#10715,#10716,#10717));
#2996=EDGE_LOOP('',(#10718,#10719,#10720,#10721));
#2997=EDGE_LOOP('',(#10722));
#2998=EDGE_LOOP('',(#10723));
#2999=EDGE_LOOP('',(#10724,#10725,#10726,#10727));
#3000=EDGE_LOOP('',(#10728));
#3001=EDGE_LOOP('',(#10729));
#3002=EDGE_LOOP('',(#10730,#10731,#10732,#10733));
#3003=EDGE_LOOP('',(#10734));
#3004=EDGE_LOOP('',(#10735));
#3005=EDGE_LOOP('',(#10736,#10737,#10738,#10739));
#3006=EDGE_LOOP('',(#10740));
#3007=EDGE_LOOP('',(#10741));
#3008=EDGE_LOOP('',(#10742,#10743,#10744,#10745));
#3009=EDGE_LOOP('',(#10746));
#3010=EDGE_LOOP('',(#10747));
#3011=EDGE_LOOP('',(#10748,#10749,#10750,#10751));
#3012=EDGE_LOOP('',(#10752));
#3013=EDGE_LOOP('',(#10753,#10754,#10755,#10756));
#3014=EDGE_LOOP('',(#10757,#10758,#10759,#10760));
#3015=EDGE_LOOP('',(#10761,#10762,#10763,#10764));
#3016=EDGE_LOOP('',(#10765));
#3017=EDGE_LOOP('',(#10766));
#3018=EDGE_LOOP('',(#10767,#10768,#10769,#10770));
#3019=EDGE_LOOP('',(#10771,#10772,#10773,#10774));
#3020=EDGE_LOOP('',(#10775,#10776,#10777,#10778));
#3021=EDGE_LOOP('',(#10779));
#3022=EDGE_LOOP('',(#10780,#10781,#10782,#10783));
#3023=EDGE_LOOP('',(#10784,#10785,#10786,#10787));
#3024=EDGE_LOOP('',(#10788,#10789,#10790,#10791));
#3025=EDGE_LOOP('',(#10792,#10793,#10794,#10795));
#3026=EDGE_LOOP('',(#10796,#10797,#10798,#10799));
#3027=EDGE_LOOP('',(#10800,#10801,#10802,#10803));
#3028=EDGE_LOOP('',(#10804,#10805,#10806,#10807,#10808,#10809));
#3029=EDGE_LOOP('',(#10810,#10811,#10812,#10813,#10814,#10815));
#3030=EDGE_LOOP('',(#10816,#10817,#10818,#10819));
#3031=EDGE_LOOP('',(#10820,#10821,#10822,#10823));
#3032=EDGE_LOOP('',(#10824,#10825));
#3033=EDGE_LOOP('',(#10826));
#3034=EDGE_LOOP('',(#10827));
#3035=EDGE_LOOP('',(#10828,#10829,#10830));
#3036=EDGE_LOOP('',(#10831,#10832,#10833));
#3037=EDGE_LOOP('',(#10834,#10835,#10836));
#3038=EDGE_LOOP('',(#10837,#10838,#10839,#10840));
#3039=EDGE_LOOP('',(#10841,#10842,#10843));
#3040=EDGE_LOOP('',(#10844,#10845,#10846,#10847));
#3041=EDGE_LOOP('',(#10848,#10849,#10850,#10851));
#3042=EDGE_LOOP('',(#10852));
#3043=EDGE_LOOP('',(#10853));
#3044=EDGE_LOOP('',(#10854,#10855,#10856,#10857,#10858,#10859,#10860,#10861,
#10862,#10863,#10864,#10865));
#3045=EDGE_LOOP('',(#10866,#10867,#10868,#10869,#10870,#10871,#10872,#10873,
#10874,#10875,#10876,#10877));
#3046=EDGE_LOOP('',(#10878,#10879));
#3047=EDGE_LOOP('',(#10880));
#3048=EDGE_LOOP('',(#10881,#10882));
#3049=EDGE_LOOP('',(#10883));
#3050=EDGE_LOOP('',(#10884,#10885,#10886,#10887));
#3051=EDGE_LOOP('',(#10888,#10889,#10890,#10891));
#3052=EDGE_LOOP('',(#10892,#10893,#10894,#10895));
#3053=EDGE_LOOP('',(#10896,#10897,#10898,#10899));
#3054=EDGE_LOOP('',(#10900,#10901,#10902,#10903));
#3055=EDGE_LOOP('',(#10904,#10905,#10906,#10907));
#3056=EDGE_LOOP('',(#10908,#10909,#10910,#10911));
#3057=EDGE_LOOP('',(#10912,#10913,#10914,#10915));
#3058=EDGE_LOOP('',(#10916,#10917,#10918,#10919));
#3059=EDGE_LOOP('',(#10920,#10921,#10922,#10923));
#3060=EDGE_LOOP('',(#10924,#10925,#10926,#10927));
#3061=EDGE_LOOP('',(#10928,#10929,#10930,#10931));
#3062=EDGE_LOOP('',(#10932,#10933,#10934,#10935));
#3063=EDGE_LOOP('',(#10936));
#3064=EDGE_LOOP('',(#10937));
#3065=EDGE_LOOP('',(#10938,#10939,#10940,#10941));
#3066=EDGE_LOOP('',(#10942));
#3067=EDGE_LOOP('',(#10943));
#3068=EDGE_LOOP('',(#10944,#10945));
#3069=EDGE_LOOP('',(#10946));
#3070=EDGE_LOOP('',(#10947));
#3071=EDGE_LOOP('',(#10948));
#3072=EDGE_LOOP('',(#10949));
#3073=EDGE_LOOP('',(#10950,#10951,#10952,#10953,#10954,#10955));
#3074=EDGE_LOOP('',(#10956,#10957,#10958,#10959,#10960,#10961));
#3075=EDGE_LOOP('',(#10962,#10963,#10964,#10965));
#3076=EDGE_LOOP('',(#10966,#10967,#10968));
#3077=EDGE_LOOP('',(#10969,#10970,#10971));
#3078=EDGE_LOOP('',(#10972,#10973,#10974));
#3079=EDGE_LOOP('',(#10975,#10976,#10977));
#3080=EDGE_LOOP('',(#10978,#10979,#10980));
#3081=EDGE_LOOP('',(#10981,#10982,#10983));
#3082=EDGE_LOOP('',(#10984,#10985,#10986,#10987,#10988,#10989));
#3083=EDGE_LOOP('',(#10990,#10991,#10992,#10993,#10994,#10995));
#3084=EDGE_LOOP('',(#10996,#10997,#10998,#10999,#11000,#11001));
#3085=EDGE_LOOP('',(#11002,#11003,#11004,#11005,#11006,#11007));
#3086=EDGE_LOOP('',(#11008));
#3087=EDGE_LOOP('',(#11009));
#3088=EDGE_LOOP('',(#11010));
#3089=EDGE_LOOP('',(#11011));
#3090=EDGE_LOOP('',(#11012,#11013,#11014,#11015));
#3091=EDGE_LOOP('',(#11016));
#3092=EDGE_LOOP('',(#11017));
#3093=EDGE_LOOP('',(#11018,#11019,#11020,#11021));
#3094=EDGE_LOOP('',(#11022));
#3095=EDGE_LOOP('',(#11023));
#3096=EDGE_LOOP('',(#11024));
#3097=EDGE_LOOP('',(#11025));
#3098=EDGE_LOOP('',(#11026));
#3099=EDGE_LOOP('',(#11027));
#3100=EDGE_LOOP('',(#11028,#11029,#11030,#11031));
#3101=EDGE_LOOP('',(#11032,#11033,#11034,#11035));
#3102=EDGE_LOOP('',(#11036));
#3103=EDGE_LOOP('',(#11037));
#3104=EDGE_LOOP('',(#11038));
#3105=EDGE_LOOP('',(#11039));
#3106=EDGE_LOOP('',(#11040,#11041,#11042,#11043));
#3107=EDGE_LOOP('',(#11044,#11045,#11046,#11047));
#3108=EDGE_LOOP('',(#11048,#11049,#11050,#11051));
#3109=EDGE_LOOP('',(#11052,#11053,#11054,#11055));
#3110=EDGE_LOOP('',(#11056,#11057,#11058,#11059));
#3111=EDGE_LOOP('',(#11060,#11061,#11062,#11063));
#3112=EDGE_LOOP('',(#11064,#11065,#11066,#11067,#11068,#11069));
#3113=EDGE_LOOP('',(#11070,#11071,#11072,#11073,#11074,#11075));
#3114=EDGE_LOOP('',(#11076));
#3115=EDGE_LOOP('',(#11077));
#3116=EDGE_LOOP('',(#11078,#11079,#11080,#11081));
#3117=EDGE_LOOP('',(#11082,#11083,#11084,#11085));
#3118=EDGE_LOOP('',(#11086,#11087,#11088,#11089));
#3119=EDGE_LOOP('',(#11090));
#3120=EDGE_LOOP('',(#11091));
#3121=EDGE_LOOP('',(#11092,#11093,#11094,#11095));
#3122=EDGE_LOOP('',(#11096,#11097,#11098,#11099));
#3123=EDGE_LOOP('',(#11100,#11101,#11102,#11103));
#3124=EDGE_LOOP('',(#11104,#11105,#11106,#11107));
#3125=EDGE_LOOP('',(#11108,#11109,#11110,#11111));
#3126=EDGE_LOOP('',(#11112,#11113,#11114,#11115));
#3127=EDGE_LOOP('',(#11116,#11117,#11118,#11119));
#3128=EDGE_LOOP('',(#11120,#11121,#11122,#11123));
#3129=EDGE_LOOP('',(#11124,#11125,#11126,#11127,#11128,#11129));
#3130=EDGE_LOOP('',(#11130,#11131,#11132,#11133,#11134,#11135));
#3131=EDGE_LOOP('',(#11136));
#3132=EDGE_LOOP('',(#11137));
#3133=EDGE_LOOP('',(#11138,#11139,#11140,#11141));
#3134=EDGE_LOOP('',(#11142,#11143,#11144,#11145));
#3135=EDGE_LOOP('',(#11146,#11147,#11148,#11149));
#3136=EDGE_LOOP('',(#11150));
#3137=EDGE_LOOP('',(#11151));
#3138=EDGE_LOOP('',(#11152,#11153,#11154,#11155));
#3139=EDGE_LOOP('',(#11156,#11157,#11158,#11159));
#3140=EDGE_LOOP('',(#11160,#11161,#11162,#11163));
#3141=EDGE_LOOP('',(#11164));
#3142=EDGE_LOOP('',(#11165));
#3143=EDGE_LOOP('',(#11166));
#3144=EDGE_LOOP('',(#11167));
#3145=EDGE_LOOP('',(#11168));
#3146=EDGE_LOOP('',(#11169,#11170,#11171,#11172));
#3147=EDGE_LOOP('',(#11173,#11174,#11175,#11176));
#3148=EDGE_LOOP('',(#11177,#11178,#11179,#11180));
#3149=EDGE_LOOP('',(#11181));
#3150=EDGE_LOOP('',(#11182));
#3151=EDGE_LOOP('',(#11183,#11184,#11185,#11186));
#3152=EDGE_LOOP('',(#11187));
#3153=EDGE_LOOP('',(#11188));
#3154=EDGE_LOOP('',(#11189));
#3155=EDGE_LOOP('',(#11190,#11191,#11192,#11193));
#3156=EDGE_LOOP('',(#11194));
#3157=EDGE_LOOP('',(#11195));
#3158=EDGE_LOOP('',(#11196,#11197,#11198,#11199));
#3159=EDGE_LOOP('',(#11200,#11201,#11202,#11203));
#3160=EDGE_LOOP('',(#11204));
#3161=EDGE_LOOP('',(#11205));
#3162=EDGE_LOOP('',(#11206));
#3163=EDGE_LOOP('',(#11207));
#3164=EDGE_LOOP('',(#11208,#11209,#11210,#11211));
#3165=EDGE_LOOP('',(#11212,#11213,#11214,#11215));
#3166=EDGE_LOOP('',(#11216));
#3167=EDGE_LOOP('',(#11217));
#3168=EDGE_LOOP('',(#11218));
#3169=EDGE_LOOP('',(#11219));
#3170=EDGE_LOOP('',(#11220,#11221,#11222,#11223));
#3171=EDGE_LOOP('',(#11224));
#3172=EDGE_LOOP('',(#11225));
#3173=EDGE_LOOP('',(#11226,#11227,#11228,#11229));
#3174=EDGE_LOOP('',(#11230));
#3175=EDGE_LOOP('',(#11231));
#3176=EDGE_LOOP('',(#11232,#11233,#11234,#11235));
#3177=EDGE_LOOP('',(#11236,#11237,#11238,#11239));
#3178=EDGE_LOOP('',(#11240));
#3179=EDGE_LOOP('',(#11241));
#3180=EDGE_LOOP('',(#11242));
#3181=EDGE_LOOP('',(#11243));
#3182=EDGE_LOOP('',(#11244,#11245,#11246,#11247));
#3183=EDGE_LOOP('',(#11248));
#3184=EDGE_LOOP('',(#11249));
#3185=EDGE_LOOP('',(#11250,#11251));
#3186=EDGE_LOOP('',(#11252,#11253,#11254,#11255,#11256,#11257,#11258,#11259,
#11260));
#3187=EDGE_LOOP('',(#11261,#11262,#11263));
#3188=EDGE_LOOP('',(#11264,#11265));
#3189=EDGE_LOOP('',(#11266,#11267,#11268,#11269,#11270,#11271,#11272,#11273,
#11274));
#3190=EDGE_LOOP('',(#11275,#11276,#11277));
#3191=EDGE_LOOP('',(#11278,#11279,#11280,#11281));
#3192=EDGE_LOOP('',(#11282,#11283,#11284,#11285));
#3193=EDGE_LOOP('',(#11286,#11287,#11288,#11289));
#3194=EDGE_LOOP('',(#11290,#11291,#11292,#11293));
#3195=EDGE_LOOP('',(#11294,#11295));
#3196=EDGE_LOOP('',(#11296,#11297));
#3197=EDGE_LOOP('',(#11298));
#3198=EDGE_LOOP('',(#11299));
#3199=EDGE_LOOP('',(#11300));
#3200=EDGE_LOOP('',(#11301));
#3201=EDGE_LOOP('',(#11302,#11303,#11304,#11305,#11306,#11307,#11308,#11309,
#11310));
#3202=EDGE_LOOP('',(#11311,#11312,#11313,#11314,#11315,#11316,#11317));
#3203=EDGE_LOOP('',(#11318,#11319,#11320,#11321,#11322,#11323,#11324,#11325,
#11326));
#3204=EDGE_LOOP('',(#11327,#11328,#11329));
#3205=EDGE_LOOP('',(#11330,#11331,#11332));
#3206=EDGE_LOOP('',(#11333,#11334,#11335));
#3207=EDGE_LOOP('',(#11336,#11337,#11338,#11339,#11340,#11341,#11342));
#3208=EDGE_LOOP('',(#11343,#11344,#11345,#11346,#11347,#11348,#11349));
#3209=EDGE_LOOP('',(#11350,#11351,#11352,#11353,#11354,#11355,#11356,#11357,
#11358,#11359));
#3210=EDGE_LOOP('',(#11360,#11361));
#3211=EDGE_LOOP('',(#11362,#11363));
#3212=EDGE_LOOP('',(#11364,#11365));
#3213=EDGE_LOOP('',(#11366));
#3214=EDGE_LOOP('',(#11367));
#3215=EDGE_LOOP('',(#11368));
#3216=EDGE_LOOP('',(#11369,#11370,#11371,#11372,#11373,#11374,#11375,#11376,
#11377,#11378,#11379,#11380,#11381,#11382,#11383,#11384,#11385,#11386,#11387,
#11388,#11389,#11390,#11391,#11392,#11393,#11394,#11395,#11396,#11397,#11398,
#11399,#11400,#11401,#11402,#11403,#11404,#11405,#11406,#11407,#11408));
#3217=EDGE_LOOP('',(#11409,#11410,#11411,#11412));
#3218=EDGE_LOOP('',(#11413));
#3219=EDGE_LOOP('',(#11414));
#3220=EDGE_LOOP('',(#11415));
#3221=EDGE_LOOP('',(#11416,#11417,#11418,#11419,#11420,#11421,#11422,#11423,
#11424,#11425,#11426,#11427,#11428,#11429,#11430,#11431,#11432,#11433,#11434,
#11435,#11436,#11437,#11438,#11439,#11440,#11441,#11442,#11443,#11444,#11445,
#11446,#11447,#11448,#11449,#11450,#11451,#11452,#11453,#11454,#11455));
#3222=EDGE_LOOP('',(#11456,#11457,#11458,#11459));
#3223=EDGE_LOOP('',(#11460));
#3224=EDGE_LOOP('',(#11461));
#3225=EDGE_LOOP('',(#11462,#11463,#11464,#11465));
#3226=EDGE_LOOP('',(#11466,#11467,#11468,#11469));
#3227=EDGE_LOOP('',(#11470,#11471,#11472,#11473));
#3228=EDGE_LOOP('',(#11474,#11475,#11476,#11477));
#3229=EDGE_LOOP('',(#11478,#11479,#11480,#11481));
#3230=EDGE_LOOP('',(#11482,#11483,#11484,#11485));
#3231=EDGE_LOOP('',(#11486,#11487,#11488,#11489));
#3232=EDGE_LOOP('',(#11490,#11491,#11492,#11493));
#3233=EDGE_LOOP('',(#11494,#11495,#11496,#11497));
#3234=EDGE_LOOP('',(#11498,#11499,#11500,#11501));
#3235=EDGE_LOOP('',(#11502,#11503,#11504,#11505));
#3236=EDGE_LOOP('',(#11506,#11507,#11508,#11509));
#3237=EDGE_LOOP('',(#11510,#11511,#11512,#11513));
#3238=EDGE_LOOP('',(#11514,#11515,#11516,#11517));
#3239=EDGE_LOOP('',(#11518,#11519,#11520,#11521));
#3240=EDGE_LOOP('',(#11522,#11523,#11524,#11525));
#3241=EDGE_LOOP('',(#11526,#11527,#11528,#11529));
#3242=EDGE_LOOP('',(#11530,#11531,#11532,#11533));
#3243=EDGE_LOOP('',(#11534,#11535,#11536,#11537));
#3244=EDGE_LOOP('',(#11538,#11539,#11540,#11541));
#3245=EDGE_LOOP('',(#11542,#11543,#11544,#11545));
#3246=EDGE_LOOP('',(#11546,#11547,#11548,#11549));
#3247=EDGE_LOOP('',(#11550,#11551,#11552,#11553));
#3248=EDGE_LOOP('',(#11554,#11555,#11556,#11557));
#3249=EDGE_LOOP('',(#11558,#11559,#11560,#11561));
#3250=EDGE_LOOP('',(#11562,#11563,#11564,#11565));
#3251=EDGE_LOOP('',(#11566,#11567,#11568,#11569));
#3252=EDGE_LOOP('',(#11570,#11571,#11572,#11573));
#3253=EDGE_LOOP('',(#11574,#11575,#11576,#11577));
#3254=EDGE_LOOP('',(#11578,#11579,#11580,#11581));
#3255=EDGE_LOOP('',(#11582,#11583,#11584,#11585));
#3256=EDGE_LOOP('',(#11586,#11587,#11588,#11589));
#3257=EDGE_LOOP('',(#11590,#11591,#11592,#11593));
#3258=EDGE_LOOP('',(#11594,#11595,#11596,#11597));
#3259=EDGE_LOOP('',(#11598,#11599,#11600,#11601));
#3260=EDGE_LOOP('',(#11602,#11603,#11604,#11605));
#3261=EDGE_LOOP('',(#11606,#11607,#11608,#11609));
#3262=EDGE_LOOP('',(#11610,#11611,#11612,#11613));
#3263=EDGE_LOOP('',(#11614,#11615,#11616,#11617));
#3264=EDGE_LOOP('',(#11618,#11619,#11620,#11621));
#3265=EDGE_LOOP('',(#11622));
#3266=EDGE_LOOP('',(#11623));
#3267=EDGE_LOOP('',(#11624,#11625,#11626,#11627));
#3268=EDGE_LOOP('',(#11628));
#3269=EDGE_LOOP('',(#11629,#11630,#11631,#11632));
#3270=EDGE_LOOP('',(#11633));
#3271=EDGE_LOOP('',(#11634));
#3272=EDGE_LOOP('',(#11635));
#3273=EDGE_LOOP('',(#11636,#11637,#11638,#11639));
#3274=EDGE_LOOP('',(#11640,#11641,#11642,#11643));
#3275=EDGE_LOOP('',(#11644));
#3276=EDGE_LOOP('',(#11645));
#3277=EDGE_LOOP('',(#11646,#11647,#11648,#11649));
#3278=EDGE_LOOP('',(#11650,#11651,#11652,#11653));
#3279=EDGE_LOOP('',(#11654));
#3280=EDGE_LOOP('',(#11655));
#3281=EDGE_LOOP('',(#11656));
#3282=EDGE_LOOP('',(#11657));
#3283=EDGE_LOOP('',(#11658,#11659,#11660,#11661));
#3284=EDGE_LOOP('',(#11662,#11663,#11664,#11665));
#3285=EDGE_LOOP('',(#11666));
#3286=EDGE_LOOP('',(#11667));
#3287=EDGE_LOOP('',(#11668));
#3288=EDGE_LOOP('',(#11669));
#3289=EDGE_LOOP('',(#11670,#11671,#11672,#11673));
#3290=EDGE_LOOP('',(#11674));
#3291=EDGE_LOOP('',(#11675));
#3292=EDGE_LOOP('',(#11676,#11677,#11678,#11679));
#3293=EDGE_LOOP('',(#11680));
#3294=EDGE_LOOP('',(#11681));
#3295=EDGE_LOOP('',(#11682,#11683,#11684,#11685));
#3296=EDGE_LOOP('',(#11686,#11687,#11688,#11689));
#3297=EDGE_LOOP('',(#11690));
#3298=EDGE_LOOP('',(#11691));
#3299=EDGE_LOOP('',(#11692));
#3300=EDGE_LOOP('',(#11693));
#3301=EDGE_LOOP('',(#11694,#11695));
#3302=EDGE_LOOP('',(#11696,#11697,#11698,#11699,#11700,#11701,#11702,#11703,
#11704));
#3303=EDGE_LOOP('',(#11705,#11706,#11707));
#3304=EDGE_LOOP('',(#11708,#11709,#11710,#11711));
#3305=EDGE_LOOP('',(#11712,#11713,#11714,#11715));
#3306=EDGE_LOOP('',(#11716,#11717,#11718,#11719));
#3307=EDGE_LOOP('',(#11720,#11721));
#3308=EDGE_LOOP('',(#11722));
#3309=EDGE_LOOP('',(#11723));
#3310=EDGE_LOOP('',(#11724));
#3311=EDGE_LOOP('',(#11725));
#3312=EDGE_LOOP('',(#11726,#11727));
#3313=EDGE_LOOP('',(#11728,#11729,#11730,#11731,#11732,#11733,#11734,#11735,
#11736));
#3314=EDGE_LOOP('',(#11737,#11738,#11739));
#3315=EDGE_LOOP('',(#11740,#11741,#11742,#11743));
#3316=EDGE_LOOP('',(#11744,#11745,#11746,#11747));
#3317=EDGE_LOOP('',(#11748,#11749,#11750,#11751));
#3318=EDGE_LOOP('',(#11752,#11753));
#3319=EDGE_LOOP('',(#11754));
#3320=EDGE_LOOP('',(#11755));
#3321=EDGE_LOOP('',(#11756));
#3322=EDGE_LOOP('',(#11757));
#3323=EDGE_LOOP('',(#11758,#11759,#11760,#11761));
#3324=EDGE_LOOP('',(#11762,#11763,#11764,#11765));
#3325=EDGE_LOOP('',(#11766));
#3326=EDGE_LOOP('',(#11767));
#3327=EDGE_LOOP('',(#11768));
#3328=EDGE_LOOP('',(#11769));
#3329=EDGE_LOOP('',(#11770,#11771,#11772,#11773));
#3330=EDGE_LOOP('',(#11774,#11775,#11776,#11777));
#3331=EDGE_LOOP('',(#11778));
#3332=EDGE_LOOP('',(#11779));
#3333=EDGE_LOOP('',(#11780));
#3334=EDGE_LOOP('',(#11781));
#3335=EDGE_LOOP('',(#11782,#11783,#11784,#11785));
#3336=EDGE_LOOP('',(#11786,#11787,#11788,#11789));
#3337=EDGE_LOOP('',(#11790));
#3338=EDGE_LOOP('',(#11791));
#3339=EDGE_LOOP('',(#11792));
#3340=EDGE_LOOP('',(#11793));
#3341=EDGE_LOOP('',(#11794,#11795));
#3342=EDGE_LOOP('',(#11796,#11797,#11798,#11799,#11800,#11801,#11802,#11803,
#11804));
#3343=EDGE_LOOP('',(#11805,#11806,#11807));
#3344=EDGE_LOOP('',(#11808,#11809,#11810,#11811));
#3345=EDGE_LOOP('',(#11812,#11813,#11814,#11815));
#3346=EDGE_LOOP('',(#11816,#11817,#11818,#11819));
#3347=EDGE_LOOP('',(#11820,#11821));
#3348=EDGE_LOOP('',(#11822));
#3349=EDGE_LOOP('',(#11823));
#3350=EDGE_LOOP('',(#11824));
#3351=EDGE_LOOP('',(#11825));
#3352=EDGE_LOOP('',(#11826,#11827));
#3353=EDGE_LOOP('',(#11828,#11829,#11830,#11831,#11832,#11833,#11834,#11835,
#11836));
#3354=EDGE_LOOP('',(#11837,#11838,#11839));
#3355=EDGE_LOOP('',(#11840,#11841,#11842,#11843));
#3356=EDGE_LOOP('',(#11844,#11845,#11846,#11847));
#3357=EDGE_LOOP('',(#11848,#11849,#11850,#11851));
#3358=EDGE_LOOP('',(#11852,#11853));
#3359=EDGE_LOOP('',(#11854));
#3360=EDGE_LOOP('',(#11855));
#3361=EDGE_LOOP('',(#11856));
#3362=EDGE_LOOP('',(#11857));
#3363=EDGE_LOOP('',(#11858,#11859,#11860,#11861,#11862,#11863,#11864,#11865,
#11866));
#3364=EDGE_LOOP('',(#11867,#11868,#11869,#11870,#11871,#11872,#11873));
#3365=EDGE_LOOP('',(#11874,#11875,#11876,#11877,#11878,#11879,#11880,#11881,
#11882));
#3366=EDGE_LOOP('',(#11883,#11884,#11885));
#3367=EDGE_LOOP('',(#11886,#11887,#11888));
#3368=EDGE_LOOP('',(#11889,#11890,#11891));
#3369=EDGE_LOOP('',(#11892,#11893,#11894,#11895,#11896,#11897,#11898));
#3370=EDGE_LOOP('',(#11899,#11900,#11901,#11902,#11903,#11904,#11905));
#3371=EDGE_LOOP('',(#11906,#11907,#11908,#11909,#11910,#11911,#11912,#11913,
#11914,#11915));
#3372=EDGE_LOOP('',(#11916,#11917));
#3373=EDGE_LOOP('',(#11918,#11919));
#3374=EDGE_LOOP('',(#11920,#11921));
#3375=EDGE_LOOP('',(#11922));
#3376=EDGE_LOOP('',(#11923));
#3377=EDGE_LOOP('',(#11924));
#3378=EDGE_LOOP('',(#11925,#11926,#11927,#11928,#11929,#11930,#11931,#11932,
#11933,#11934,#11935,#11936,#11937,#11938,#11939,#11940,#11941,#11942,#11943,
#11944,#11945,#11946,#11947,#11948,#11949,#11950,#11951,#11952,#11953,#11954,
#11955,#11956,#11957,#11958,#11959,#11960,#11961,#11962,#11963,#11964,#11965,
#11966,#11967,#11968,#11969,#11970,#11971,#11972,#11973,#11974,#11975,#11976,
#11977,#11978,#11979,#11980,#11981,#11982,#11983,#11984,#11985,#11986,#11987,
#11988,#11989,#11990,#11991,#11992,#11993,#11994,#11995,#11996,#11997,#11998,
#11999,#12000,#12001,#12002,#12003,#12004));
#3379=EDGE_LOOP('',(#12005,#12006,#12007,#12008));
#3380=EDGE_LOOP('',(#12009));
#3381=EDGE_LOOP('',(#12010));
#3382=EDGE_LOOP('',(#12011));
#3383=EDGE_LOOP('',(#12012,#12013,#12014,#12015,#12016,#12017,#12018,#12019,
#12020,#12021,#12022,#12023,#12024,#12025,#12026,#12027,#12028,#12029,#12030,
#12031,#12032,#12033,#12034,#12035,#12036,#12037,#12038,#12039,#12040,#12041,
#12042,#12043,#12044,#12045,#12046,#12047,#12048,#12049,#12050,#12051,#12052,
#12053,#12054,#12055,#12056,#12057,#12058,#12059,#12060,#12061,#12062,#12063,
#12064,#12065,#12066,#12067,#12068,#12069,#12070,#12071,#12072,#12073,#12074,
#12075,#12076,#12077,#12078,#12079,#12080,#12081,#12082,#12083,#12084,#12085,
#12086,#12087,#12088,#12089,#12090,#12091));
#3384=EDGE_LOOP('',(#12092,#12093,#12094,#12095));
#3385=EDGE_LOOP('',(#12096));
#3386=EDGE_LOOP('',(#12097));
#3387=EDGE_LOOP('',(#12098,#12099,#12100,#12101));
#3388=EDGE_LOOP('',(#12102,#12103,#12104,#12105));
#3389=EDGE_LOOP('',(#12106,#12107,#12108,#12109));
#3390=EDGE_LOOP('',(#12110,#12111,#12112,#12113));
#3391=EDGE_LOOP('',(#12114,#12115,#12116,#12117));
#3392=EDGE_LOOP('',(#12118,#12119,#12120,#12121));
#3393=EDGE_LOOP('',(#12122,#12123,#12124,#12125));
#3394=EDGE_LOOP('',(#12126,#12127,#12128,#12129));
#3395=EDGE_LOOP('',(#12130,#12131,#12132,#12133));
#3396=EDGE_LOOP('',(#12134,#12135,#12136,#12137));
#3397=EDGE_LOOP('',(#12138,#12139,#12140,#12141));
#3398=EDGE_LOOP('',(#12142,#12143,#12144,#12145));
#3399=EDGE_LOOP('',(#12146,#12147,#12148,#12149));
#3400=EDGE_LOOP('',(#12150,#12151,#12152,#12153));
#3401=EDGE_LOOP('',(#12154,#12155,#12156,#12157));
#3402=EDGE_LOOP('',(#12158,#12159,#12160,#12161));
#3403=EDGE_LOOP('',(#12162,#12163,#12164,#12165));
#3404=EDGE_LOOP('',(#12166,#12167,#12168,#12169));
#3405=EDGE_LOOP('',(#12170,#12171,#12172,#12173));
#3406=EDGE_LOOP('',(#12174,#12175,#12176,#12177));
#3407=EDGE_LOOP('',(#12178,#12179,#12180,#12181));
#3408=EDGE_LOOP('',(#12182,#12183,#12184,#12185));
#3409=EDGE_LOOP('',(#12186,#12187,#12188,#12189));
#3410=EDGE_LOOP('',(#12190,#12191,#12192,#12193));
#3411=EDGE_LOOP('',(#12194,#12195,#12196,#12197));
#3412=EDGE_LOOP('',(#12198,#12199,#12200,#12201));
#3413=EDGE_LOOP('',(#12202,#12203,#12204,#12205));
#3414=EDGE_LOOP('',(#12206,#12207,#12208,#12209));
#3415=EDGE_LOOP('',(#12210,#12211,#12212,#12213));
#3416=EDGE_LOOP('',(#12214,#12215,#12216,#12217));
#3417=EDGE_LOOP('',(#12218,#12219,#12220,#12221));
#3418=EDGE_LOOP('',(#12222,#12223,#12224,#12225));
#3419=EDGE_LOOP('',(#12226,#12227,#12228,#12229));
#3420=EDGE_LOOP('',(#12230,#12231,#12232,#12233));
#3421=EDGE_LOOP('',(#12234,#12235,#12236,#12237));
#3422=EDGE_LOOP('',(#12238,#12239,#12240,#12241));
#3423=EDGE_LOOP('',(#12242,#12243,#12244,#12245));
#3424=EDGE_LOOP('',(#12246,#12247,#12248,#12249));
#3425=EDGE_LOOP('',(#12250,#12251,#12252,#12253));
#3426=EDGE_LOOP('',(#12254,#12255,#12256,#12257));
#3427=EDGE_LOOP('',(#12258,#12259,#12260,#12261));
#3428=EDGE_LOOP('',(#12262,#12263,#12264,#12265));
#3429=EDGE_LOOP('',(#12266,#12267,#12268,#12269));
#3430=EDGE_LOOP('',(#12270,#12271,#12272,#12273));
#3431=EDGE_LOOP('',(#12274,#12275,#12276,#12277));
#3432=EDGE_LOOP('',(#12278,#12279,#12280,#12281));
#3433=EDGE_LOOP('',(#12282,#12283,#12284,#12285));
#3434=EDGE_LOOP('',(#12286,#12287,#12288,#12289));
#3435=EDGE_LOOP('',(#12290,#12291,#12292,#12293));
#3436=EDGE_LOOP('',(#12294,#12295,#12296,#12297));
#3437=EDGE_LOOP('',(#12298,#12299,#12300,#12301));
#3438=EDGE_LOOP('',(#12302,#12303,#12304,#12305));
#3439=EDGE_LOOP('',(#12306,#12307,#12308,#12309));
#3440=EDGE_LOOP('',(#12310,#12311,#12312,#12313));
#3441=EDGE_LOOP('',(#12314,#12315,#12316,#12317));
#3442=EDGE_LOOP('',(#12318,#12319,#12320,#12321));
#3443=EDGE_LOOP('',(#12322,#12323,#12324,#12325));
#3444=EDGE_LOOP('',(#12326,#12327,#12328,#12329));
#3445=EDGE_LOOP('',(#12330,#12331,#12332,#12333));
#3446=EDGE_LOOP('',(#12334,#12335,#12336,#12337));
#3447=EDGE_LOOP('',(#12338,#12339,#12340,#12341));
#3448=EDGE_LOOP('',(#12342,#12343,#12344,#12345));
#3449=EDGE_LOOP('',(#12346,#12347,#12348,#12349));
#3450=EDGE_LOOP('',(#12350,#12351,#12352,#12353));
#3451=EDGE_LOOP('',(#12354,#12355,#12356,#12357));
#3452=EDGE_LOOP('',(#12358,#12359,#12360,#12361));
#3453=EDGE_LOOP('',(#12362,#12363,#12364,#12365));
#3454=EDGE_LOOP('',(#12366,#12367,#12368,#12369));
#3455=EDGE_LOOP('',(#12370,#12371,#12372,#12373));
#3456=EDGE_LOOP('',(#12374,#12375,#12376,#12377));
#3457=EDGE_LOOP('',(#12378,#12379,#12380,#12381));
#3458=EDGE_LOOP('',(#12382,#12383,#12384,#12385));
#3459=EDGE_LOOP('',(#12386,#12387,#12388,#12389));
#3460=EDGE_LOOP('',(#12390,#12391,#12392,#12393));
#3461=EDGE_LOOP('',(#12394,#12395,#12396,#12397));
#3462=EDGE_LOOP('',(#12398,#12399,#12400,#12401));
#3463=EDGE_LOOP('',(#12402,#12403,#12404,#12405));
#3464=EDGE_LOOP('',(#12406,#12407,#12408,#12409));
#3465=EDGE_LOOP('',(#12410,#12411,#12412,#12413));
#3466=EDGE_LOOP('',(#12414,#12415,#12416,#12417));
#3467=EDGE_LOOP('',(#12418));
#3468=EDGE_LOOP('',(#12419,#12420,#12421,#12422));
#3469=EDGE_LOOP('',(#12423,#12424,#12425,#12426));
#3470=EDGE_LOOP('',(#12427,#12428,#12429,#12430));
#3471=EDGE_LOOP('',(#12431));
#3472=EDGE_LOOP('',(#12432));
#3473=EDGE_LOOP('',(#12433,#12434,#12435,#12436));
#3474=EDGE_LOOP('',(#12437,#12438,#12439,#12440));
#3475=EDGE_LOOP('',(#12441,#12442,#12443,#12444));
#3476=EDGE_LOOP('',(#12445));
#3477=EDGE_LOOP('',(#12446,#12447,#12448,#12449));
#3478=EDGE_LOOP('',(#12450,#12451,#12452,#12453));
#3479=EDGE_LOOP('',(#12454,#12455,#12456,#12457));
#3480=EDGE_LOOP('',(#12458,#12459,#12460,#12461));
#3481=EDGE_LOOP('',(#12462,#12463,#12464,#12465));
#3482=EDGE_LOOP('',(#12466,#12467,#12468,#12469));
#3483=EDGE_LOOP('',(#12470,#12471,#12472,#12473,#12474,#12475));
#3484=EDGE_LOOP('',(#12476,#12477,#12478,#12479,#12480,#12481));
#3485=EDGE_LOOP('',(#12482,#12483,#12484,#12485));
#3486=EDGE_LOOP('',(#12486,#12487,#12488,#12489));
#3487=EDGE_LOOP('',(#12490,#12491,#12492,#12493));
#3488=EDGE_LOOP('',(#12494,#12495,#12496,#12497));
#3489=EDGE_LOOP('',(#12498,#12499,#12500,#12501));
#3490=EDGE_LOOP('',(#12502,#12503,#12504,#12505));
#3491=EDGE_LOOP('',(#12506,#12507,#12508,#12509,#12510,#12511));
#3492=EDGE_LOOP('',(#12512));
#3493=EDGE_LOOP('',(#12513,#12514,#12515,#12516,#12517,#12518));
#3494=EDGE_LOOP('',(#12519,#12520,#12521,#12522));
#3495=EDGE_LOOP('',(#12523,#12524,#12525,#12526));
#3496=EDGE_LOOP('',(#12527,#12528,#12529,#12530));
#3497=EDGE_LOOP('',(#12531));
#3498=LINE('',#20977,#4290);
#3499=LINE('',#20984,#4291);
#3500=LINE('',#20991,#4292);
#3501=LINE('',#20998,#4293);
#3502=LINE('',#21005,#4294);
#3503=LINE('',#21012,#4295);
#3504=LINE('',#21019,#4296);
#3505=LINE('',#21026,#4297);
#3506=LINE('',#21033,#4298);
#3507=LINE('',#21040,#4299);
#3508=LINE('',#21046,#4300);
#3509=LINE('',#21050,#4301);
#3510=LINE('',#21055,#4302);
#3511=LINE('',#21059,#4303);
#3512=LINE('',#21064,#4304);
#3513=LINE('',#21066,#4305);
#3514=LINE('',#21068,#4306);
#3515=LINE('',#21069,#4307);
#3516=LINE('',#21074,#4308);
#3517=LINE('',#21077,#4309);
#3518=LINE('',#21082,#4310);
#3519=LINE('',#21085,#4311);
#3520=LINE('',#21090,#4312);
#3521=LINE('',#21093,#4313);
#3522=LINE('',#21094,#4314);
#3523=LINE('',#21095,#4315);
#3524=LINE('',#21097,#4316);
#3525=LINE('',#21099,#4317);
#3526=LINE('',#21102,#4318);
#3527=LINE('',#21104,#4319);
#3528=LINE('',#21108,#4320);
#3529=LINE('',#21111,#4321);
#3530=LINE('',#21113,#4322);
#3531=LINE('',#21115,#4323);
#3532=LINE('',#21119,#4324);
#3533=LINE('',#21122,#4325);
#3534=LINE('',#21124,#4326);
#3535=LINE('',#21128,#4327);
#3536=LINE('',#21132,#4328);
#3537=LINE('',#21135,#4329);
#3538=LINE('',#21137,#4330);
#3539=LINE('',#21139,#4331);
#3540=LINE('',#21143,#4332);
#3541=LINE('',#21146,#4333);
#3542=LINE('',#21148,#4334);
#3543=LINE('',#21152,#4335);
#3544=LINE('',#21156,#4336);
#3545=LINE('',#21159,#4337);
#3546=LINE('',#21161,#4338);
#3547=LINE('',#21163,#4339);
#3548=LINE('',#21172,#4340);
#3549=LINE('',#21179,#4341);
#3550=LINE('',#21188,#4342);
#3551=LINE('',#21190,#4343);
#3552=LINE('',#21191,#4344);
#3553=LINE('',#21194,#4345);
#3554=LINE('',#21195,#4346);
#3555=LINE('',#21198,#4347);
#3556=LINE('',#21199,#4348);
#3557=LINE('',#21201,#4349);
#3558=LINE('',#21207,#4350);
#3559=LINE('',#21209,#4351);
#3560=LINE('',#21211,#4352);
#3561=LINE('',#21212,#4353);
#3562=LINE('',#21215,#4354);
#3563=LINE('',#21217,#4355);
#3564=LINE('',#21218,#4356);
#3565=LINE('',#21221,#4357);
#3566=LINE('',#21223,#4358);
#3567=LINE('',#21224,#4359);
#3568=LINE('',#21226,#4360);
#3569=LINE('',#21227,#4361);
#3570=LINE('',#21234,#4362);
#3571=LINE('',#21236,#4363);
#3572=LINE('',#21238,#4364);
#3573=LINE('',#21239,#4365);
#3574=LINE('',#21242,#4366);
#3575=LINE('',#21244,#4367);
#3576=LINE('',#21245,#4368);
#3577=LINE('',#21248,#4369);
#3578=LINE('',#21250,#4370);
#3579=LINE('',#21251,#4371);
#3580=LINE('',#21253,#4372);
#3581=LINE('',#21254,#4373);
#3582=LINE('',#21262,#4374);
#3583=LINE('',#21268,#4375);
#3584=LINE('',#21274,#4376);
#3585=LINE('',#21280,#4377);
#3586=LINE('',#21286,#4378);
#3587=LINE('',#21292,#4379);
#3588=LINE('',#21298,#4380);
#3589=LINE('',#21304,#4381);
#3590=LINE('',#21310,#4382);
#3591=LINE('',#21315,#4383);
#3592=LINE('',#21317,#4384);
#3593=LINE('',#21319,#4385);
#3594=LINE('',#21320,#4386);
#3595=LINE('',#21324,#4387);
#3596=LINE('',#21326,#4388);
#3597=LINE('',#21328,#4389);
#3598=LINE('',#21329,#4390);
#3599=LINE('',#21332,#4391);
#3600=LINE('',#21334,#4392);
#3601=LINE('',#21335,#4393);
#3602=LINE('',#21338,#4394);
#3603=LINE('',#21340,#4395);
#3604=LINE('',#21341,#4396);
#3605=LINE('',#21344,#4397);
#3606=LINE('',#21346,#4398);
#3607=LINE('',#21347,#4399);
#3608=LINE('',#21348,#4400);
#3609=LINE('',#21351,#4401);
#3610=LINE('',#21352,#4402);
#3611=LINE('',#21355,#4403);
#3612=LINE('',#21356,#4404);
#3613=LINE('',#21357,#4405);
#3614=LINE('',#21359,#4406);
#3615=LINE('',#21367,#4407);
#3616=LINE('',#21373,#4408);
#3617=LINE('',#21381,#4409);
#3618=LINE('',#21385,#4410);
#3619=LINE('',#21390,#4411);
#3620=LINE('',#21394,#4412);
#3621=LINE('',#21399,#4413);
#3622=LINE('',#21403,#4414);
#3623=LINE('',#21408,#4415);
#3624=LINE('',#21412,#4416);
#3625=LINE('',#21433,#4417);
#3626=LINE('',#21439,#4418);
#3627=LINE('',#21445,#4419);
#3628=LINE('',#21449,#4420);
#3629=LINE('',#21454,#4421);
#3630=LINE('',#21458,#4422);
#3631=LINE('',#21463,#4423);
#3632=LINE('',#21467,#4424);
#3633=LINE('',#21472,#4425);
#3634=LINE('',#21476,#4426);
#3635=LINE('',#21495,#4427);
#3636=LINE('',#21503,#4428);
#3637=LINE('',#21509,#4429);
#3638=LINE('',#21513,#4430);
#3639=LINE('',#21518,#4431);
#3640=LINE('',#21522,#4432);
#3641=LINE('',#21526,#4433);
#3642=LINE('',#21529,#4434);
#3643=LINE('',#21530,#4435);
#3644=LINE('',#21543,#4436);
#3645=LINE('',#21546,#4437);
#3646=LINE('',#21549,#4438);
#3647=LINE('',#21551,#4439);
#3648=LINE('',#21553,#4440);
#3649=LINE('',#21555,#4441);
#3650=LINE('',#21556,#4442);
#3651=LINE('',#21559,#4443);
#3652=LINE('',#21561,#4444);
#3653=LINE('',#21562,#4445);
#3654=LINE('',#21563,#4446);
#3655=LINE('',#21566,#4447);
#3656=LINE('',#21570,#4448);
#3657=LINE('',#21574,#4449);
#3658=LINE('',#21578,#4450);
#3659=LINE('',#21582,#4451);
#3660=LINE('',#21586,#4452);
#3661=LINE('',#21591,#4453);
#3662=LINE('',#21597,#4454);
#3663=LINE('',#21603,#4455);
#3664=LINE('',#21609,#4456);
#3665=LINE('',#21613,#4457);
#3666=LINE('',#21615,#4458);
#3667=LINE('',#21616,#4459);
#3668=LINE('',#21620,#4460);
#3669=LINE('',#21622,#4461);
#3670=LINE('',#21624,#4462);
#3671=LINE('',#21625,#4463);
#3672=LINE('',#21628,#4464);
#3673=LINE('',#21630,#4465);
#3674=LINE('',#21631,#4466);
#3675=LINE('',#21634,#4467);
#3676=LINE('',#21636,#4468);
#3677=LINE('',#21637,#4469);
#3678=LINE('',#21639,#4470);
#3679=LINE('',#21640,#4471);
#3680=LINE('',#21642,#4472);
#3681=LINE('',#21643,#4473);
#3682=LINE('',#21651,#4474);
#3683=LINE('',#21657,#4475);
#3684=LINE('',#21666,#4476);
#3685=LINE('',#21672,#4477);
#3686=LINE('',#21681,#4478);
#3687=LINE('',#21687,#4479);
#3688=LINE('',#21696,#4480);
#3689=LINE('',#21702,#4481);
#3690=LINE('',#21711,#4482);
#3691=LINE('',#21717,#4483);
#3692=LINE('',#21725,#4484);
#3693=LINE('',#21729,#4485);
#3694=LINE('',#21734,#4486);
#3695=LINE('',#21738,#4487);
#3696=LINE('',#21743,#4488);
#3697=LINE('',#21747,#4489);
#3698=LINE('',#21752,#4490);
#3699=LINE('',#21756,#4491);
#3700=LINE('',#21777,#4492);
#3701=LINE('',#21783,#4493);
#3702=LINE('',#21789,#4494);
#3703=LINE('',#21793,#4495);
#3704=LINE('',#21812,#4496);
#3705=LINE('',#21815,#4497);
#3706=LINE('',#21827,#4498);
#3707=LINE('',#21830,#4499);
#3708=LINE('',#21842,#4500);
#3709=LINE('',#21845,#4501);
#3710=LINE('',#21848,#4502);
#3711=LINE('',#21851,#4503);
#3712=LINE('',#21854,#4504);
#3713=LINE('',#21857,#4505);
#3714=LINE('',#21860,#4506);
#3715=LINE('',#21863,#4507);
#3716=LINE('',#21868,#4508);
#3717=LINE('',#21886,#4509);
#3718=LINE('',#21889,#4510);
#3719=LINE('',#21894,#4511);
#3720=LINE('',#21896,#4512);
#3721=LINE('',#21898,#4513);
#3722=LINE('',#21899,#4514);
#3723=LINE('',#21903,#4515);
#3724=LINE('',#21905,#4516);
#3725=LINE('',#21907,#4517);
#3726=LINE('',#21908,#4518);
#3727=LINE('',#21912,#4519);
#3728=LINE('',#21916,#4520);
#3729=LINE('',#21926,#4521);
#3730=LINE('',#21929,#4522);
#3731=LINE('',#21932,#4523);
#3732=LINE('',#21933,#4524);
#3733=LINE('',#21936,#4525);
#3734=LINE('',#21937,#4526);
#3735=LINE('',#21946,#4527);
#3736=LINE('',#21954,#4528);
#3737=LINE('',#21959,#4529);
#3738=LINE('',#21967,#4530);
#3739=LINE('',#21972,#4531);
#3740=LINE('',#21980,#4532);
#3741=LINE('',#21985,#4533);
#3742=LINE('',#21993,#4534);
#3743=LINE('',#21998,#4535);
#3744=LINE('',#22005,#4536);
#3745=LINE('',#22011,#4537);
#3746=LINE('',#22013,#4538);
#3747=LINE('',#22015,#4539);
#3748=LINE('',#22016,#4540);
#3749=LINE('',#22019,#4541);
#3750=LINE('',#22021,#4542);
#3751=LINE('',#22022,#4543);
#3752=LINE('',#22025,#4544);
#3753=LINE('',#22027,#4545);
#3754=LINE('',#22028,#4546);
#3755=LINE('',#22030,#4547);
#3756=LINE('',#22031,#4548);
#3757=LINE('',#22039,#4549);
#3758=LINE('',#22045,#4550);
#3759=LINE('',#22054,#4551);
#3760=LINE('',#22060,#4552);
#3761=LINE('',#22069,#4553);
#3762=LINE('',#22077,#4554);
#3763=LINE('',#22082,#4555);
#3764=LINE('',#22090,#4556);
#3765=LINE('',#22095,#4557);
#3766=LINE('',#22103,#4558);
#3767=LINE('',#22108,#4559);
#3768=LINE('',#22116,#4560);
#3769=LINE('',#22121,#4561);
#3770=LINE('',#22128,#4562);
#3771=LINE('',#22134,#4563);
#3772=LINE('',#22136,#4564);
#3773=LINE('',#22138,#4565);
#3774=LINE('',#22139,#4566);
#3775=LINE('',#22142,#4567);
#3776=LINE('',#22144,#4568);
#3777=LINE('',#22145,#4569);
#3778=LINE('',#22148,#4570);
#3779=LINE('',#22150,#4571);
#3780=LINE('',#22151,#4572);
#3781=LINE('',#22153,#4573);
#3782=LINE('',#22154,#4574);
#3783=LINE('',#22162,#4575);
#3784=LINE('',#22168,#4576);
#3785=LINE('',#22177,#4577);
#3786=LINE('',#22183,#4578);
#3787=LINE('',#22192,#4579);
#3788=LINE('',#22200,#4580);
#3789=LINE('',#22205,#4581);
#3790=LINE('',#22213,#4582);
#3791=LINE('',#22217,#4583);
#3792=LINE('',#22219,#4584);
#3793=LINE('',#22221,#4585);
#3794=LINE('',#22222,#4586);
#3795=LINE('',#22225,#4587);
#3796=LINE('',#22227,#4588);
#3797=LINE('',#22228,#4589);
#3798=LINE('',#22231,#4590);
#3799=LINE('',#22233,#4591);
#3800=LINE('',#22234,#4592);
#3801=LINE('',#22236,#4593);
#3802=LINE('',#22237,#4594);
#3803=LINE('',#22244,#4595);
#3804=LINE('',#22246,#4596);
#3805=LINE('',#22248,#4597);
#3806=LINE('',#22249,#4598);
#3807=LINE('',#22252,#4599);
#3808=LINE('',#22254,#4600);
#3809=LINE('',#22255,#4601);
#3810=LINE('',#22258,#4602);
#3811=LINE('',#22260,#4603);
#3812=LINE('',#22261,#4604);
#3813=LINE('',#22263,#4605);
#3814=LINE('',#22264,#4606);
#3815=LINE('',#22272,#4607);
#3816=LINE('',#22278,#4608);
#3817=LINE('',#22283,#4609);
#3818=LINE('',#22285,#4610);
#3819=LINE('',#22287,#4611);
#3820=LINE('',#22288,#4612);
#3821=LINE('',#22291,#4613);
#3822=LINE('',#22293,#4614);
#3823=LINE('',#22294,#4615);
#3824=LINE('',#22297,#4616);
#3825=LINE('',#22299,#4617);
#3826=LINE('',#22300,#4618);
#3827=LINE('',#22302,#4619);
#3828=LINE('',#22303,#4620);
#3829=LINE('',#22311,#4621);
#3830=LINE('',#22317,#4622);
#3831=LINE('',#22322,#4623);
#3832=LINE('',#22324,#4624);
#3833=LINE('',#22326,#4625);
#3834=LINE('',#22327,#4626);
#3835=LINE('',#22330,#4627);
#3836=LINE('',#22332,#4628);
#3837=LINE('',#22333,#4629);
#3838=LINE('',#22336,#4630);
#3839=LINE('',#22338,#4631);
#3840=LINE('',#22339,#4632);
#3841=LINE('',#22341,#4633);
#3842=LINE('',#22342,#4634);
#3843=LINE('',#22350,#4635);
#3844=LINE('',#22356,#4636);
#3845=LINE('',#22362,#4637);
#3846=LINE('',#22368,#4638);
#3847=LINE('',#22373,#4639);
#3848=LINE('',#22375,#4640);
#3849=LINE('',#22377,#4641);
#3850=LINE('',#22378,#4642);
#3851=LINE('',#22381,#4643);
#3852=LINE('',#22383,#4644);
#3853=LINE('',#22384,#4645);
#3854=LINE('',#22387,#4646);
#3855=LINE('',#22389,#4647);
#3856=LINE('',#22390,#4648);
#3857=LINE('',#22392,#4649);
#3858=LINE('',#22393,#4650);
#3859=LINE('',#22410,#4651);
#3860=LINE('',#22416,#4652);
#3861=LINE('',#22420,#4653);
#3862=LINE('',#22426,#4654);
#3863=LINE('',#22431,#4655);
#3864=LINE('',#22446,#4656);
#3865=LINE('',#22455,#4657);
#3866=LINE('',#22459,#4658);
#3867=LINE('',#22463,#4659);
#3868=LINE('',#22466,#4660);
#3869=LINE('',#22619,#4661);
#3870=LINE('',#22915,#4662);
#3871=LINE('',#22957,#4663);
#3872=LINE('',#22962,#4664);
#3873=LINE('',#22971,#4665);
#3874=LINE('',#22976,#4666);
#3875=LINE('',#22986,#4667);
#3876=LINE('',#22988,#4668);
#3877=LINE('',#22990,#4669);
#3878=LINE('',#22991,#4670);
#3879=LINE('',#22994,#4671);
#3880=LINE('',#22996,#4672);
#3881=LINE('',#22997,#4673);
#3882=LINE('',#23000,#4674);
#3883=LINE('',#23002,#4675);
#3884=LINE('',#23003,#4676);
#3885=LINE('',#23006,#4677);
#3886=LINE('',#23008,#4678);
#3887=LINE('',#23009,#4679);
#3888=LINE('',#23012,#4680);
#3889=LINE('',#23014,#4681);
#3890=LINE('',#23015,#4682);
#3891=LINE('',#23017,#4683);
#3892=LINE('',#23018,#4684);
#3893=LINE('',#23028,#4685);
#3894=LINE('',#23037,#4686);
#3895=LINE('',#23041,#4687);
#3896=LINE('',#23045,#4688);
#3897=LINE('',#23052,#4689);
#3898=LINE('',#23056,#4690);
#3899=LINE('',#23058,#4691);
#3900=LINE('',#23073,#4692);
#3901=LINE('',#23079,#4693);
#3902=LINE('',#23083,#4694);
#3903=LINE('',#23089,#4695);
#3904=LINE('',#23094,#4696);
#3905=LINE('',#23109,#4697);
#3906=LINE('',#23118,#4698);
#3907=LINE('',#23122,#4699);
#3908=LINE('',#23126,#4700);
#3909=LINE('',#23129,#4701);
#3910=LINE('',#23265,#4702);
#3911=LINE('',#23518,#4703);
#3912=LINE('',#23560,#4704);
#3913=LINE('',#23565,#4705);
#3914=LINE('',#23574,#4706);
#3915=LINE('',#23579,#4707);
#3916=LINE('',#23592,#4708);
#3917=LINE('',#23596,#4709);
#3918=LINE('',#23600,#4710);
#3919=LINE('',#23607,#4711);
#3920=LINE('',#23611,#4712);
#3921=LINE('',#23615,#4713);
#3922=LINE('',#23620,#4714);
#3923=LINE('',#23622,#4715);
#3924=LINE('',#23624,#4716);
#3925=LINE('',#23625,#4717);
#3926=LINE('',#23628,#4718);
#3927=LINE('',#23630,#4719);
#3928=LINE('',#23631,#4720);
#3929=LINE('',#23634,#4721);
#3930=LINE('',#23636,#4722);
#3931=LINE('',#23637,#4723);
#3932=LINE('',#23640,#4724);
#3933=LINE('',#23642,#4725);
#3934=LINE('',#23643,#4726);
#3935=LINE('',#23646,#4727);
#3936=LINE('',#23648,#4728);
#3937=LINE('',#23649,#4729);
#3938=LINE('',#23651,#4730);
#3939=LINE('',#23652,#4731);
#3940=LINE('',#23661,#4732);
#3941=LINE('',#23667,#4733);
#3942=LINE('',#23676,#4734);
#3943=LINE('',#23678,#4735);
#3944=LINE('',#23683,#4736);
#3945=LINE('',#23686,#4737);
#3946=LINE('',#23690,#4738);
#3947=LINE('',#23693,#4739);
#3948=LINE('',#23695,#4740);
#3949=LINE('',#23696,#4741);
#3950=LINE('',#23700,#4742);
#3951=LINE('',#23702,#4743);
#3952=LINE('',#23705,#4744);
#3953=LINE('',#23706,#4745);
#3954=LINE('',#23710,#4746);
#3955=LINE('',#23712,#4747);
#3956=LINE('',#23714,#4748);
#3957=LINE('',#23715,#4749);
#3958=LINE('',#23721,#4750);
#3959=LINE('',#23723,#4751);
#3960=LINE('',#23724,#4752);
#3961=LINE('',#23726,#4753);
#3962=LINE('',#23728,#4754);
#3963=LINE('',#23729,#4755);
#3964=LINE('',#23738,#4756);
#3965=LINE('',#23740,#4757);
#3966=LINE('',#23742,#4758);
#3967=LINE('',#23743,#4759);
#3968=LINE('',#23746,#4760);
#3969=LINE('',#23748,#4761);
#3970=LINE('',#23749,#4762);
#3971=LINE('',#23752,#4763);
#3972=LINE('',#23754,#4764);
#3973=LINE('',#23755,#4765);
#3974=LINE('',#23757,#4766);
#3975=LINE('',#23758,#4767);
#3976=LINE('',#23763,#4768);
#3977=LINE('',#23767,#4769);
#3978=LINE('',#23771,#4770);
#3979=LINE('',#23772,#4771);
#3980=LINE('',#23773,#4772);
#3981=LINE('',#23776,#4773);
#3982=LINE('',#23777,#4774);
#3983=LINE('',#23780,#4775);
#3984=LINE('',#23781,#4776);
#3985=LINE('',#23783,#4777);
#3986=LINE('',#23790,#4778);
#3987=LINE('',#23845,#4779);
#3988=LINE('',#23917,#4780);
#3989=LINE('',#23962,#4781);
#3990=LINE('',#24130,#4782);
#3991=LINE('',#24201,#4783);
#3992=LINE('',#24204,#4784);
#3993=LINE('',#24275,#4785);
#3994=LINE('',#24285,#4786);
#3995=LINE('',#24290,#4787);
#3996=LINE('',#24298,#4788);
#3997=LINE('',#24304,#4789);
#3998=LINE('',#24312,#4790);
#3999=LINE('',#24314,#4791);
#4000=LINE('',#24316,#4792);
#4001=LINE('',#24317,#4793);
#4002=LINE('',#24320,#4794);
#4003=LINE('',#24322,#4795);
#4004=LINE('',#24323,#4796);
#4005=LINE('',#24326,#4797);
#4006=LINE('',#24328,#4798);
#4007=LINE('',#24329,#4799);
#4008=LINE('',#24332,#4800);
#4009=LINE('',#24334,#4801);
#4010=LINE('',#24335,#4802);
#4011=LINE('',#24338,#4803);
#4012=LINE('',#24340,#4804);
#4013=LINE('',#24341,#4805);
#4014=LINE('',#24343,#4806);
#4015=LINE('',#24344,#4807);
#4016=LINE('',#24356,#4808);
#4017=LINE('',#24360,#4809);
#4018=LINE('',#24364,#4810);
#4019=LINE('',#24371,#4811);
#4020=LINE('',#24373,#4812);
#4021=LINE('',#24378,#4813);
#4022=LINE('',#24380,#4814);
#4023=LINE('',#24382,#4815);
#4024=LINE('',#24383,#4816);
#4025=LINE('',#24386,#4817);
#4026=LINE('',#24388,#4818);
#4027=LINE('',#24389,#4819);
#4028=LINE('',#24392,#4820);
#4029=LINE('',#24394,#4821);
#4030=LINE('',#24395,#4822);
#4031=LINE('',#24398,#4823);
#4032=LINE('',#24400,#4824);
#4033=LINE('',#24401,#4825);
#4034=LINE('',#24404,#4826);
#4035=LINE('',#24406,#4827);
#4036=LINE('',#24407,#4828);
#4037=LINE('',#24409,#4829);
#4038=LINE('',#24410,#4830);
#4039=LINE('',#24422,#4831);
#4040=LINE('',#24426,#4832);
#4041=LINE('',#24430,#4833);
#4042=LINE('',#24437,#4834);
#4043=LINE('',#24439,#4835);
#4044=LINE('',#24446,#4836);
#4045=LINE('',#24460,#4837);
#4046=LINE('',#24463,#4838);
#4047=LINE('',#24469,#4839);
#4048=LINE('',#24475,#4840);
#4049=LINE('',#24483,#4841);
#4050=LINE('',#24490,#4842);
#4051=LINE('',#24496,#4843);
#4052=LINE('',#24505,#4844);
#4053=LINE('',#24511,#4845);
#4054=LINE('',#24520,#4846);
#4055=LINE('',#24529,#4847);
#4056=LINE('',#24538,#4848);
#4057=LINE('',#24544,#4849);
#4058=LINE('',#24553,#4850);
#4059=LINE('',#24561,#4851);
#4060=LINE('',#24578,#4852);
#4061=LINE('',#24629,#4853);
#4062=LINE('',#24633,#4854);
#4063=LINE('',#24650,#4855);
#4064=LINE('',#24701,#4856);
#4065=LINE('',#24706,#4857);
#4066=LINE('',#24712,#4858);
#4067=LINE('',#24760,#4859);
#4068=LINE('',#24844,#4860);
#4069=LINE('',#24888,#4861);
#4070=LINE('',#24890,#4862);
#4071=LINE('',#24976,#4863);
#4072=LINE('',#25053,#4864);
#4073=LINE('',#25057,#4865);
#4074=LINE('',#25059,#4866);
#4075=LINE('',#25148,#4867);
#4076=LINE('',#25236,#4868);
#4077=LINE('',#25239,#4869);
#4078=LINE('',#25240,#4870);
#4079=LINE('',#25242,#4871);
#4080=LINE('',#25244,#4872);
#4081=LINE('',#25246,#4873);
#4082=LINE('',#25248,#4874);
#4083=LINE('',#25250,#4875);
#4084=LINE('',#25252,#4876);
#4085=LINE('',#25254,#4877);
#4086=LINE('',#25256,#4878);
#4087=LINE('',#25258,#4879);
#4088=LINE('',#25260,#4880);
#4089=LINE('',#25262,#4881);
#4090=LINE('',#25264,#4882);
#4091=LINE('',#25266,#4883);
#4092=LINE('',#25268,#4884);
#4093=LINE('',#25270,#4885);
#4094=LINE('',#25272,#4886);
#4095=LINE('',#25274,#4887);
#4096=LINE('',#25276,#4888);
#4097=LINE('',#25278,#4889);
#4098=LINE('',#25280,#4890);
#4099=LINE('',#25282,#4891);
#4100=LINE('',#25284,#4892);
#4101=LINE('',#25286,#4893);
#4102=LINE('',#25288,#4894);
#4103=LINE('',#25290,#4895);
#4104=LINE('',#25292,#4896);
#4105=LINE('',#25294,#4897);
#4106=LINE('',#25296,#4898);
#4107=LINE('',#25298,#4899);
#4108=LINE('',#25300,#4900);
#4109=LINE('',#25302,#4901);
#4110=LINE('',#25304,#4902);
#4111=LINE('',#25306,#4903);
#4112=LINE('',#25308,#4904);
#4113=LINE('',#25310,#4905);
#4114=LINE('',#25312,#4906);
#4115=LINE('',#25314,#4907);
#4116=LINE('',#25316,#4908);
#4117=LINE('',#25328,#4909);
#4118=LINE('',#25334,#4910);
#4119=LINE('',#25343,#4911);
#4120=LINE('',#25346,#4912);
#4121=LINE('',#25354,#4913);
#4122=LINE('',#25360,#4914);
#4123=LINE('',#25369,#4915);
#4124=LINE('',#25375,#4916);
#4125=LINE('',#25384,#4917);
#4126=LINE('',#25393,#4918);
#4127=LINE('',#25402,#4919);
#4128=LINE('',#25408,#4920);
#4129=LINE('',#25416,#4921);
#4130=LINE('',#25437,#4922);
#4131=LINE('',#25492,#4923);
#4132=LINE('',#25497,#4924);
#4133=LINE('',#25503,#4925);
#4134=LINE('',#25511,#4926);
#4135=LINE('',#25532,#4927);
#4136=LINE('',#25587,#4928);
#4137=LINE('',#25592,#4929);
#4138=LINE('',#25598,#4930);
#4139=LINE('',#25607,#4931);
#4140=LINE('',#25613,#4932);
#4141=LINE('',#25622,#4933);
#4142=LINE('',#25628,#4934);
#4143=LINE('',#25637,#4935);
#4144=LINE('',#25643,#4936);
#4145=LINE('',#25651,#4937);
#4146=LINE('',#25672,#4938);
#4147=LINE('',#25727,#4939);
#4148=LINE('',#25732,#4940);
#4149=LINE('',#25738,#4941);
#4150=LINE('',#25746,#4942);
#4151=LINE('',#25767,#4943);
#4152=LINE('',#25822,#4944);
#4153=LINE('',#25827,#4945);
#4154=LINE('',#25833,#4946);
#4155=LINE('',#25881,#4947);
#4156=LINE('',#25965,#4948);
#4157=LINE('',#26009,#4949);
#4158=LINE('',#26011,#4950);
#4159=LINE('',#26097,#4951);
#4160=LINE('',#26174,#4952);
#4161=LINE('',#26178,#4953);
#4162=LINE('',#26180,#4954);
#4163=LINE('',#26349,#4955);
#4164=LINE('',#26517,#4956);
#4165=LINE('',#26520,#4957);
#4166=LINE('',#26521,#4958);
#4167=LINE('',#26523,#4959);
#4168=LINE('',#26525,#4960);
#4169=LINE('',#26527,#4961);
#4170=LINE('',#26529,#4962);
#4171=LINE('',#26531,#4963);
#4172=LINE('',#26533,#4964);
#4173=LINE('',#26535,#4965);
#4174=LINE('',#26537,#4966);
#4175=LINE('',#26539,#4967);
#4176=LINE('',#26541,#4968);
#4177=LINE('',#26543,#4969);
#4178=LINE('',#26545,#4970);
#4179=LINE('',#26547,#4971);
#4180=LINE('',#26549,#4972);
#4181=LINE('',#26551,#4973);
#4182=LINE('',#26553,#4974);
#4183=LINE('',#26555,#4975);
#4184=LINE('',#26557,#4976);
#4185=LINE('',#26559,#4977);
#4186=LINE('',#26561,#4978);
#4187=LINE('',#26563,#4979);
#4188=LINE('',#26565,#4980);
#4189=LINE('',#26567,#4981);
#4190=LINE('',#26569,#4982);
#4191=LINE('',#26571,#4983);
#4192=LINE('',#26573,#4984);
#4193=LINE('',#26575,#4985);
#4194=LINE('',#26577,#4986);
#4195=LINE('',#26579,#4987);
#4196=LINE('',#26581,#4988);
#4197=LINE('',#26583,#4989);
#4198=LINE('',#26585,#4990);
#4199=LINE('',#26587,#4991);
#4200=LINE('',#26589,#4992);
#4201=LINE('',#26591,#4993);
#4202=LINE('',#26593,#4994);
#4203=LINE('',#26595,#4995);
#4204=LINE('',#26597,#4996);
#4205=LINE('',#26599,#4997);
#4206=LINE('',#26601,#4998);
#4207=LINE('',#26603,#4999);
#4208=LINE('',#26605,#5000);
#4209=LINE('',#26607,#5001);
#4210=LINE('',#26609,#5002);
#4211=LINE('',#26611,#5003);
#4212=LINE('',#26613,#5004);
#4213=LINE('',#26615,#5005);
#4214=LINE('',#26617,#5006);
#4215=LINE('',#26619,#5007);
#4216=LINE('',#26621,#5008);
#4217=LINE('',#26623,#5009);
#4218=LINE('',#26625,#5010);
#4219=LINE('',#26627,#5011);
#4220=LINE('',#26629,#5012);
#4221=LINE('',#26631,#5013);
#4222=LINE('',#26633,#5014);
#4223=LINE('',#26635,#5015);
#4224=LINE('',#26637,#5016);
#4225=LINE('',#26639,#5017);
#4226=LINE('',#26641,#5018);
#4227=LINE('',#26643,#5019);
#4228=LINE('',#26645,#5020);
#4229=LINE('',#26647,#5021);
#4230=LINE('',#26649,#5022);
#4231=LINE('',#26651,#5023);
#4232=LINE('',#26653,#5024);
#4233=LINE('',#26655,#5025);
#4234=LINE('',#26657,#5026);
#4235=LINE('',#26659,#5027);
#4236=LINE('',#26661,#5028);
#4237=LINE('',#26663,#5029);
#4238=LINE('',#26665,#5030);
#4239=LINE('',#26667,#5031);
#4240=LINE('',#26669,#5032);
#4241=LINE('',#26671,#5033);
#4242=LINE('',#26673,#5034);
#4243=LINE('',#26675,#5035);
#4244=LINE('',#26677,#5036);
#4245=LINE('',#26686,#5037);
#4246=LINE('',#26690,#5038);
#4247=LINE('',#26694,#5039);
#4248=LINE('',#26701,#5040);
#4249=LINE('',#26705,#5041);
#4250=LINE('',#26709,#5042);
#4251=LINE('',#26714,#5043);
#4252=LINE('',#26716,#5044);
#4253=LINE('',#26718,#5045);
#4254=LINE('',#26719,#5046);
#4255=LINE('',#26722,#5047);
#4256=LINE('',#26724,#5048);
#4257=LINE('',#26725,#5049);
#4258=LINE('',#26728,#5050);
#4259=LINE('',#26730,#5051);
#4260=LINE('',#26731,#5052);
#4261=LINE('',#26734,#5053);
#4262=LINE('',#26736,#5054);
#4263=LINE('',#26737,#5055);
#4264=LINE('',#26740,#5056);
#4265=LINE('',#26742,#5057);
#4266=LINE('',#26743,#5058);
#4267=LINE('',#26745,#5059);
#4268=LINE('',#26746,#5060);
#4269=LINE('',#26832,#5061);
#4270=LINE('',#26834,#5062);
#4271=LINE('',#26836,#5063);
#4272=LINE('',#26837,#5064);
#4273=LINE('',#26840,#5065);
#4274=LINE('',#26842,#5066);
#4275=LINE('',#26843,#5067);
#4276=LINE('',#26846,#5068);
#4277=LINE('',#26848,#5069);
#4278=LINE('',#26849,#5070);
#4279=LINE('',#26852,#5071);
#4280=LINE('',#26854,#5072);
#4281=LINE('',#26855,#5073);
#4282=LINE('',#26858,#5074);
#4283=LINE('',#26860,#5075);
#4284=LINE('',#26861,#5076);
#4285=LINE('',#26863,#5077);
#4286=LINE('',#26864,#5078);
#4287=LINE('',#26872,#5079);
#4288=LINE('',#26876,#5080);
#4289=LINE('',#26880,#5081);
#4290=VECTOR('',#16444,0.165);
#4291=VECTOR('',#16453,0.165);
#4292=VECTOR('',#16462,0.210000000000001);
#4293=VECTOR('',#16471,0.210000000000001);
#4294=VECTOR('',#16480,0.21);
#4295=VECTOR('',#16489,0.21);
#4296=VECTOR('',#16498,0.210000000000001);
#4297=VECTOR('',#16507,0.210000000000001);
#4298=VECTOR('',#16516,0.21);
#4299=VECTOR('',#16525,0.21);
#4300=VECTOR('',#16532,1.);
#4301=VECTOR('',#16535,1.);
#4302=VECTOR('',#16540,1.);
#4303=VECTOR('',#16543,1.);
#4304=VECTOR('',#16548,1.);
#4305=VECTOR('',#16549,1.);
#4306=VECTOR('',#16550,1.);
#4307=VECTOR('',#16551,1.);
#4308=VECTOR('',#16554,1.);
#4309=VECTOR('',#16557,1.);
#4310=VECTOR('',#16560,1.);
#4311=VECTOR('',#16563,1.);
#4312=VECTOR('',#16566,1.);
#4313=VECTOR('',#16569,1.);
#4314=VECTOR('',#16570,1.);
#4315=VECTOR('',#16571,1.);
#4316=VECTOR('',#16574,1.);
#4317=VECTOR('',#16577,1.);
#4318=VECTOR('',#16580,1.);
#4319=VECTOR('',#16581,1.);
#4320=VECTOR('',#16586,1.);
#4321=VECTOR('',#16589,1.);
#4322=VECTOR('',#16592,1.);
#4323=VECTOR('',#16595,1.);
#4324=VECTOR('',#16598,1.);
#4325=VECTOR('',#16601,1.);
#4326=VECTOR('',#16602,1.);
#4327=VECTOR('',#16605,1.);
#4328=VECTOR('',#16610,1.);
#4329=VECTOR('',#16613,1.);
#4330=VECTOR('',#16616,1.);
#4331=VECTOR('',#16619,1.);
#4332=VECTOR('',#16622,1.);
#4333=VECTOR('',#16625,1.);
#4334=VECTOR('',#16626,1.);
#4335=VECTOR('',#16629,1.);
#4336=VECTOR('',#16634,1.);
#4337=VECTOR('',#16637,1.);
#4338=VECTOR('',#16640,1.);
#4339=VECTOR('',#16643,1.);
#4340=VECTOR('',#16656,0.165);
#4341=VECTOR('',#16665,0.165);
#4342=VECTOR('',#16680,1.);
#4343=VECTOR('',#16681,1.);
#4344=VECTOR('',#16682,1.);
#4345=VECTOR('',#16685,1.);
#4346=VECTOR('',#16686,1.);
#4347=VECTOR('',#16689,1.);
#4348=VECTOR('',#16690,1.);
#4349=VECTOR('',#16693,1.);
#4350=VECTOR('',#16700,1.);
#4351=VECTOR('',#16701,1.);
#4352=VECTOR('',#16702,1.);
#4353=VECTOR('',#16703,1.);
#4354=VECTOR('',#16706,1.);
#4355=VECTOR('',#16707,1.);
#4356=VECTOR('',#16708,1.);
#4357=VECTOR('',#16711,1.);
#4358=VECTOR('',#16712,1.);
#4359=VECTOR('',#16713,1.);
#4360=VECTOR('',#16716,1.);
#4361=VECTOR('',#16717,1.);
#4362=VECTOR('',#16726,1.);
#4363=VECTOR('',#16727,1.);
#4364=VECTOR('',#16728,1.);
#4365=VECTOR('',#16729,1.);
#4366=VECTOR('',#16732,1.);
#4367=VECTOR('',#16733,1.);
#4368=VECTOR('',#16734,1.);
#4369=VECTOR('',#16737,1.);
#4370=VECTOR('',#16738,1.);
#4371=VECTOR('',#16739,1.);
#4372=VECTOR('',#16742,1.);
#4373=VECTOR('',#16743,1.);
#4374=VECTOR('',#16754,0.165);
#4375=VECTOR('',#16761,0.165);
#4376=VECTOR('',#16768,0.165);
#4377=VECTOR('',#16775,0.165);
#4378=VECTOR('',#16782,1.5);
#4379=VECTOR('',#16789,0.225);
#4380=VECTOR('',#16796,0.225);
#4381=VECTOR('',#16803,0.225);
#4382=VECTOR('',#16810,0.225);
#4383=VECTOR('',#16815,1.);
#4384=VECTOR('',#16816,1.);
#4385=VECTOR('',#16817,1.);
#4386=VECTOR('',#16818,1.);
#4387=VECTOR('',#16821,1.);
#4388=VECTOR('',#16822,1.);
#4389=VECTOR('',#16823,1.);
#4390=VECTOR('',#16824,1.);
#4391=VECTOR('',#16827,1.);
#4392=VECTOR('',#16828,1.);
#4393=VECTOR('',#16829,1.);
#4394=VECTOR('',#16832,1.);
#4395=VECTOR('',#16833,1.);
#4396=VECTOR('',#16834,1.);
#4397=VECTOR('',#16837,1.);
#4398=VECTOR('',#16838,1.);
#4399=VECTOR('',#16839,1.);
#4400=VECTOR('',#16840,1.);
#4401=VECTOR('',#16843,1.);
#4402=VECTOR('',#16844,1.);
#4403=VECTOR('',#16847,1.);
#4404=VECTOR('',#16848,1.);
#4405=VECTOR('',#16849,1.);
#4406=VECTOR('',#16852,1.);
#4407=VECTOR('',#16863,1.1);
#4408=VECTOR('',#16870,1.49);
#4409=VECTOR('',#16881,1.);
#4410=VECTOR('',#16884,1.);
#4411=VECTOR('',#16889,1.);
#4412=VECTOR('',#16892,1.);
#4413=VECTOR('',#16897,1.);
#4414=VECTOR('',#16900,1.);
#4415=VECTOR('',#16905,1.);
#4416=VECTOR('',#16908,1.);
#4417=VECTOR('',#16943,1.49);
#4418=VECTOR('',#16952,1.1);
#4419=VECTOR('',#16959,1.);
#4420=VECTOR('',#16962,1.);
#4421=VECTOR('',#16967,1.);
#4422=VECTOR('',#16970,1.);
#4423=VECTOR('',#16975,1.);
#4424=VECTOR('',#16978,1.);
#4425=VECTOR('',#16983,1.);
#4426=VECTOR('',#16986,1.);
#4427=VECTOR('',#17019,1.49);
#4428=VECTOR('',#17030,1.1);
#4429=VECTOR('',#17037,1.);
#4430=VECTOR('',#17040,1.);
#4431=VECTOR('',#17045,1.);
#4432=VECTOR('',#17048,1.);
#4433=VECTOR('',#17053,1.);
#4434=VECTOR('',#17056,1.);
#4435=VECTOR('',#17057,1.);
#4436=VECTOR('',#17070,1.);
#4437=VECTOR('',#17073,1.);
#4438=VECTOR('',#17076,1.);
#4439=VECTOR('',#17077,1.);
#4440=VECTOR('',#17078,1.);
#4441=VECTOR('',#17079,1.);
#4442=VECTOR('',#17080,1.);
#4443=VECTOR('',#17083,1.);
#4444=VECTOR('',#17084,1.);
#4445=VECTOR('',#17085,1.);
#4446=VECTOR('',#17086,1.);
#4447=VECTOR('',#17091,1.);
#4448=VECTOR('',#17096,0.165);
#4449=VECTOR('',#17101,0.165);
#4450=VECTOR('',#17106,0.164999999999999);
#4451=VECTOR('',#17111,0.164999999999999);
#4452=VECTOR('',#17116,1.6);
#4453=VECTOR('',#17121,0.225);
#4454=VECTOR('',#17128,0.225);
#4455=VECTOR('',#17135,0.225);
#4456=VECTOR('',#17142,0.225);
#4457=VECTOR('',#17147,1.);
#4458=VECTOR('',#17148,1.);
#4459=VECTOR('',#17149,1.);
#4460=VECTOR('',#17152,1.);
#4461=VECTOR('',#17153,1.);
#4462=VECTOR('',#17154,1.);
#4463=VECTOR('',#17155,1.);
#4464=VECTOR('',#17158,1.);
#4465=VECTOR('',#17159,1.);
#4466=VECTOR('',#17160,1.);
#4467=VECTOR('',#17163,1.);
#4468=VECTOR('',#17164,1.);
#4469=VECTOR('',#17165,1.);
#4470=VECTOR('',#17168,1.);
#4471=VECTOR('',#17169,1.);
#4472=VECTOR('',#17172,1.);
#4473=VECTOR('',#17173,1.);
#4474=VECTOR('',#17184,0.165);
#4475=VECTOR('',#17191,0.4);
#4476=VECTOR('',#17204,0.165);
#4477=VECTOR('',#17211,0.4);
#4478=VECTOR('',#17224,0.164999999999999);
#4479=VECTOR('',#17231,0.4);
#4480=VECTOR('',#17244,0.164999999999999);
#4481=VECTOR('',#17251,0.4);
#4482=VECTOR('',#17264,1.2);
#4483=VECTOR('',#17271,1.59);
#4484=VECTOR('',#17282,1.);
#4485=VECTOR('',#17285,1.);
#4486=VECTOR('',#17290,1.);
#4487=VECTOR('',#17293,1.);
#4488=VECTOR('',#17298,1.);
#4489=VECTOR('',#17301,1.);
#4490=VECTOR('',#17306,1.);
#4491=VECTOR('',#17309,1.);
#4492=VECTOR('',#17344,1.59);
#4493=VECTOR('',#17353,1.2);
#4494=VECTOR('',#17360,1.);
#4495=VECTOR('',#17363,1.);
#4496=VECTOR('',#17386,1.);
#4497=VECTOR('',#17389,1.);
#4498=VECTOR('',#17402,1.);
#4499=VECTOR('',#17405,1.);
#4500=VECTOR('',#17418,1.);
#4501=VECTOR('',#17421,1.);
#4502=VECTOR('',#17424,1.);
#4503=VECTOR('',#17427,1.);
#4504=VECTOR('',#17430,1.);
#4505=VECTOR('',#17433,1.);
#4506=VECTOR('',#17436,1.);
#4507=VECTOR('',#17439,1.);
#4508=VECTOR('',#17446,1.);
#4509=VECTOR('',#17475,1.);
#4510=VECTOR('',#17480,1.2);
#4511=VECTOR('',#17485,1.);
#4512=VECTOR('',#17486,1.);
#4513=VECTOR('',#17487,1.);
#4514=VECTOR('',#17488,1.);
#4515=VECTOR('',#17491,1.);
#4516=VECTOR('',#17492,1.);
#4517=VECTOR('',#17493,1.);
#4518=VECTOR('',#17494,1.);
#4519=VECTOR('',#17497,1.);
#4520=VECTOR('',#17500,1.);
#4521=VECTOR('',#17517,1.);
#4522=VECTOR('',#17520,1.);
#4523=VECTOR('',#17523,1.);
#4524=VECTOR('',#17524,1.);
#4525=VECTOR('',#17527,1.);
#4526=VECTOR('',#17528,1.);
#4527=VECTOR('',#17541,0.475);
#4528=VECTOR('',#17552,0.275);
#4529=VECTOR('',#17557,0.475);
#4530=VECTOR('',#17568,0.275);
#4531=VECTOR('',#17573,0.475);
#4532=VECTOR('',#17584,0.275);
#4533=VECTOR('',#17589,0.475);
#4534=VECTOR('',#17600,0.275);
#4535=VECTOR('',#17605,0.34);
#4536=VECTOR('',#17614,0.34);
#4537=VECTOR('',#17621,1.);
#4538=VECTOR('',#17622,1.);
#4539=VECTOR('',#17623,1.);
#4540=VECTOR('',#17624,1.);
#4541=VECTOR('',#17627,1.);
#4542=VECTOR('',#17628,1.);
#4543=VECTOR('',#17629,1.);
#4544=VECTOR('',#17632,1.);
#4545=VECTOR('',#17633,1.);
#4546=VECTOR('',#17634,1.);
#4547=VECTOR('',#17637,1.);
#4548=VECTOR('',#17638,1.);
#4549=VECTOR('',#17649,0.425);
#4550=VECTOR('',#17656,0.645);
#4551=VECTOR('',#17669,0.425000000000001);
#4552=VECTOR('',#17676,0.645);
#4553=VECTOR('',#17689,0.475);
#4554=VECTOR('',#17700,0.275);
#4555=VECTOR('',#17705,0.475);
#4556=VECTOR('',#17716,0.275);
#4557=VECTOR('',#17721,0.475);
#4558=VECTOR('',#17732,0.275);
#4559=VECTOR('',#17737,0.475);
#4560=VECTOR('',#17748,0.275);
#4561=VECTOR('',#17753,0.34);
#4562=VECTOR('',#17762,0.34);
#4563=VECTOR('',#17769,1.);
#4564=VECTOR('',#17770,1.);
#4565=VECTOR('',#17771,1.);
#4566=VECTOR('',#17772,1.);
#4567=VECTOR('',#17775,1.);
#4568=VECTOR('',#17776,1.);
#4569=VECTOR('',#17777,1.);
#4570=VECTOR('',#17780,1.);
#4571=VECTOR('',#17781,1.);
#4572=VECTOR('',#17782,1.);
#4573=VECTOR('',#17785,1.);
#4574=VECTOR('',#17786,1.);
#4575=VECTOR('',#17797,0.425);
#4576=VECTOR('',#17804,0.645);
#4577=VECTOR('',#17817,0.425000000000001);
#4578=VECTOR('',#17824,0.645);
#4579=VECTOR('',#17837,0.4);
#4580=VECTOR('',#17848,0.225);
#4581=VECTOR('',#17853,0.4);
#4582=VECTOR('',#17864,0.225);
#4583=VECTOR('',#17867,1.);
#4584=VECTOR('',#17868,1.);
#4585=VECTOR('',#17869,1.);
#4586=VECTOR('',#17870,1.);
#4587=VECTOR('',#17873,1.);
#4588=VECTOR('',#17874,1.);
#4589=VECTOR('',#17875,1.);
#4590=VECTOR('',#17878,1.);
#4591=VECTOR('',#17879,1.);
#4592=VECTOR('',#17880,1.);
#4593=VECTOR('',#17883,1.);
#4594=VECTOR('',#17884,1.);
#4595=VECTOR('',#17893,1.);
#4596=VECTOR('',#17894,1.);
#4597=VECTOR('',#17895,1.);
#4598=VECTOR('',#17896,1.);
#4599=VECTOR('',#17899,1.);
#4600=VECTOR('',#17900,1.);
#4601=VECTOR('',#17901,1.);
#4602=VECTOR('',#17904,1.);
#4603=VECTOR('',#17905,1.);
#4604=VECTOR('',#17906,1.);
#4605=VECTOR('',#17909,1.);
#4606=VECTOR('',#17910,1.);
#4607=VECTOR('',#17921,0.165);
#4608=VECTOR('',#17928,0.165);
#4609=VECTOR('',#17933,1.);
#4610=VECTOR('',#17934,1.);
#4611=VECTOR('',#17935,1.);
#4612=VECTOR('',#17936,1.);
#4613=VECTOR('',#17939,1.);
#4614=VECTOR('',#17940,1.);
#4615=VECTOR('',#17941,1.);
#4616=VECTOR('',#17944,1.);
#4617=VECTOR('',#17945,1.);
#4618=VECTOR('',#17946,1.);
#4619=VECTOR('',#17949,1.);
#4620=VECTOR('',#17950,1.);
#4621=VECTOR('',#17961,0.164999999999999);
#4622=VECTOR('',#17968,0.164999999999999);
#4623=VECTOR('',#17973,1.);
#4624=VECTOR('',#17974,1.);
#4625=VECTOR('',#17975,1.);
#4626=VECTOR('',#17976,1.);
#4627=VECTOR('',#17979,1.);
#4628=VECTOR('',#17980,1.);
#4629=VECTOR('',#17981,1.);
#4630=VECTOR('',#17984,1.);
#4631=VECTOR('',#17985,1.);
#4632=VECTOR('',#17986,1.);
#4633=VECTOR('',#17989,1.);
#4634=VECTOR('',#17990,1.);
#4635=VECTOR('',#18001,0.225);
#4636=VECTOR('',#18008,0.225);
#4637=VECTOR('',#18015,0.225);
#4638=VECTOR('',#18022,0.225);
#4639=VECTOR('',#18027,1.);
#4640=VECTOR('',#18028,1.);
#4641=VECTOR('',#18029,1.);
#4642=VECTOR('',#18030,1.);
#4643=VECTOR('',#18033,1.);
#4644=VECTOR('',#18034,1.);
#4645=VECTOR('',#18035,1.);
#4646=VECTOR('',#18038,1.);
#4647=VECTOR('',#18039,1.);
#4648=VECTOR('',#18040,1.);
#4649=VECTOR('',#18043,1.);
#4650=VECTOR('',#18044,1.);
#4651=VECTOR('',#18067,0.976185);
#4652=VECTOR('',#18074,0.5);
#4653=VECTOR('',#18079,0.53);
#4654=VECTOR('',#18088,0.976185);
#4655=VECTOR('',#18095,0.53);
#4656=VECTOR('',#18114,1.023815);
#4657=VECTOR('',#18125,1.47);
#4658=VECTOR('',#18130,1.5);
#4659=VECTOR('',#18135,1.47);
#4660=VECTOR('',#18140,1.023815);
#4661=VECTOR('',#18191,1.019052);
#4662=VECTOR('',#18268,0.980948);
#4663=VECTOR('',#18297,1.013815);
#4664=VECTOR('',#18304,0.991185);
#4665=VECTOR('',#18315,1.013815);
#4666=VECTOR('',#18322,0.991185);
#4667=VECTOR('',#18337,1.);
#4668=VECTOR('',#18338,1.);
#4669=VECTOR('',#18339,1.);
#4670=VECTOR('',#18340,1.);
#4671=VECTOR('',#18343,1.);
#4672=VECTOR('',#18344,1.);
#4673=VECTOR('',#18345,1.);
#4674=VECTOR('',#18348,1.);
#4675=VECTOR('',#18349,1.);
#4676=VECTOR('',#18350,1.);
#4677=VECTOR('',#18353,1.);
#4678=VECTOR('',#18354,1.);
#4679=VECTOR('',#18355,1.);
#4680=VECTOR('',#18358,1.);
#4681=VECTOR('',#18359,1.);
#4682=VECTOR('',#18360,1.);
#4683=VECTOR('',#18363,1.);
#4684=VECTOR('',#18364,1.);
#4685=VECTOR('',#18377,0.2);
#4686=VECTOR('',#18390,0.325);
#4687=VECTOR('',#18395,0.35);
#4688=VECTOR('',#18400,0.335);
#4689=VECTOR('',#18409,0.21);
#4690=VECTOR('',#18414,0.2);
#4691=VECTOR('',#18417,0.18);
#4692=VECTOR('',#18436,1.070235);
#4693=VECTOR('',#18443,0.6);
#4694=VECTOR('',#18448,0.63);
#4695=VECTOR('',#18457,1.070235);
#4696=VECTOR('',#18464,0.63);
#4697=VECTOR('',#18483,1.129765);
#4698=VECTOR('',#18494,1.57);
#4699=VECTOR('',#18499,1.6);
#4700=VECTOR('',#18504,1.57);
#4701=VECTOR('',#18509,1.129765);
#4702=VECTOR('',#18556,1.123812);
#4703=VECTOR('',#18625,1.076188);
#4704=VECTOR('',#18654,1.119765);
#4705=VECTOR('',#18661,1.085235);
#4706=VECTOR('',#18672,1.119765);
#4707=VECTOR('',#18679,1.085235);
#4708=VECTOR('',#18700,0.4);
#4709=VECTOR('',#18705,0.425);
#4710=VECTOR('',#18710,0.41);
#4711=VECTOR('',#18719,0.26);
#4712=VECTOR('',#18724,0.25);
#4713=VECTOR('',#18729,0.225);
#4714=VECTOR('',#18734,1.);
#4715=VECTOR('',#18735,1.);
#4716=VECTOR('',#18736,1.);
#4717=VECTOR('',#18737,1.);
#4718=VECTOR('',#18740,1.);
#4719=VECTOR('',#18741,1.);
#4720=VECTOR('',#18742,1.);
#4721=VECTOR('',#18745,1.);
#4722=VECTOR('',#18746,1.);
#4723=VECTOR('',#18747,1.);
#4724=VECTOR('',#18750,1.);
#4725=VECTOR('',#18751,1.);
#4726=VECTOR('',#18752,1.);
#4727=VECTOR('',#18755,1.);
#4728=VECTOR('',#18756,1.);
#4729=VECTOR('',#18757,1.);
#4730=VECTOR('',#18760,1.);
#4731=VECTOR('',#18761,1.);
#4732=VECTOR('',#18774,2.05);
#4733=VECTOR('',#18781,2.05);
#4734=VECTOR('',#18790,1.);
#4735=VECTOR('',#18791,1.);
#4736=VECTOR('',#18796,1.);
#4737=VECTOR('',#18799,1.);
#4738=VECTOR('',#18802,1.);
#4739=VECTOR('',#18805,1.);
#4740=VECTOR('',#18808,1.);
#4741=VECTOR('',#18809,1.);
#4742=VECTOR('',#18812,1.);
#4743=VECTOR('',#18813,1.);
#4744=VECTOR('',#18818,1.);
#4745=VECTOR('',#18819,1.);
#4746=VECTOR('',#18822,1.);
#4747=VECTOR('',#18823,1.);
#4748=VECTOR('',#18824,1.);
#4749=VECTOR('',#18825,1.);
#4750=VECTOR('',#18830,1.);
#4751=VECTOR('',#18831,1.);
#4752=VECTOR('',#18832,1.);
#4753=VECTOR('',#18833,1.);
#4754=VECTOR('',#18834,1.);
#4755=VECTOR('',#18835,1.);
#4756=VECTOR('',#18848,1.);
#4757=VECTOR('',#18849,1.);
#4758=VECTOR('',#18850,1.);
#4759=VECTOR('',#18851,1.);
#4760=VECTOR('',#18854,1.);
#4761=VECTOR('',#18855,1.);
#4762=VECTOR('',#18856,1.);
#4763=VECTOR('',#18859,1.);
#4764=VECTOR('',#18860,1.);
#4765=VECTOR('',#18861,1.);
#4766=VECTOR('',#18864,1.);
#4767=VECTOR('',#18865,1.);
#4768=VECTOR('',#18872,0.65);
#4769=VECTOR('',#18877,0.65);
#4770=VECTOR('',#18880,1.);
#4771=VECTOR('',#18881,1.);
#4772=VECTOR('',#18882,1.);
#4773=VECTOR('',#18885,1.);
#4774=VECTOR('',#18886,1.);
#4775=VECTOR('',#18889,1.);
#4776=VECTOR('',#18890,1.);
#4777=VECTOR('',#18893,1.);
#4778=VECTOR('',#18902,1.8);
#4779=VECTOR('',#18919,0.25);
#4780=VECTOR('',#18922,0.25);
#4781=VECTOR('',#18927,1.65);
#4782=VECTOR('',#18932,0.25);
#4783=VECTOR('',#18935,0.25);
#4784=VECTOR('',#18938,0.25);
#4785=VECTOR('',#18941,0.25);
#4786=VECTOR('',#18954,1.75);
#4787=VECTOR('',#18961,1.);
#4788=VECTOR('',#18972,0.42);
#4789=VECTOR('',#18979,0.8);
#4790=VECTOR('',#18990,1.);
#4791=VECTOR('',#18991,1.);
#4792=VECTOR('',#18992,1.);
#4793=VECTOR('',#18993,1.);
#4794=VECTOR('',#18996,1.);
#4795=VECTOR('',#18997,1.);
#4796=VECTOR('',#18998,1.);
#4797=VECTOR('',#19001,1.);
#4798=VECTOR('',#19002,1.);
#4799=VECTOR('',#19003,1.);
#4800=VECTOR('',#19006,1.);
#4801=VECTOR('',#19007,1.);
#4802=VECTOR('',#19008,1.);
#4803=VECTOR('',#19011,1.);
#4804=VECTOR('',#19012,1.);
#4805=VECTOR('',#19013,1.);
#4806=VECTOR('',#19016,1.);
#4807=VECTOR('',#19017,1.);
#4808=VECTOR('',#19034,0.625);
#4809=VECTOR('',#19039,0.65);
#4810=VECTOR('',#19044,0.635);
#4811=VECTOR('',#19053,0.41);
#4812=VECTOR('',#19056,0.4);
#4813=VECTOR('',#19061,1.);
#4814=VECTOR('',#19062,1.);
#4815=VECTOR('',#19063,1.);
#4816=VECTOR('',#19064,1.);
#4817=VECTOR('',#19067,1.);
#4818=VECTOR('',#19068,1.);
#4819=VECTOR('',#19069,1.);
#4820=VECTOR('',#19072,1.);
#4821=VECTOR('',#19073,1.);
#4822=VECTOR('',#19074,1.);
#4823=VECTOR('',#19077,1.);
#4824=VECTOR('',#19078,1.);
#4825=VECTOR('',#19079,1.);
#4826=VECTOR('',#19082,1.);
#4827=VECTOR('',#19083,1.);
#4828=VECTOR('',#19084,1.);
#4829=VECTOR('',#19087,1.);
#4830=VECTOR('',#19088,1.);
#4831=VECTOR('',#19105,0.325);
#4832=VECTOR('',#19110,0.35);
#4833=VECTOR('',#19115,0.335);
#4834=VECTOR('',#19124,0.21);
#4835=VECTOR('',#19127,0.2);
#4836=VECTOR('',#19136,0.165);
#4837=VECTOR('',#19155,0.7);
#4838=VECTOR('',#19158,0.5);
#4839=VECTOR('',#19165,0.4);
#4840=VECTOR('',#19174,0.5);
#4841=VECTOR('',#19185,0.505);
#4842=VECTOR('',#19194,0.405);
#4843=VECTOR('',#19201,0.7);
#4844=VECTOR('',#19214,0.505);
#4845=VECTOR('',#19221,0.7);
#4846=VECTOR('',#19234,0.15);
#4847=VECTOR('',#19247,0.15);
#4848=VECTOR('',#19260,0.225);
#4849=VECTOR('',#19267,0.6);
#4850=VECTOR('',#19280,0.5);
#4851=VECTOR('',#19291,1.);
#4852=VECTOR('',#19298,0.21);
#4853=VECTOR('',#19303,1.);
#4854=VECTOR('',#19306,1.);
#4855=VECTOR('',#19313,0.21);
#4856=VECTOR('',#19318,1.);
#4857=VECTOR('',#19323,0.505);
#4858=VECTOR('',#19330,1.);
#4859=VECTOR('',#19341,0.125);
#4860=VECTOR('',#19344,0.125);
#4861=VECTOR('',#19349,0.65);
#4862=VECTOR('',#19350,0.65);
#4863=VECTOR('',#19355,0.125);
#4864=VECTOR('',#19358,0.125);
#4865=VECTOR('',#19363,0.4);
#4866=VECTOR('',#19364,0.4);
#4867=VECTOR('',#19457,0.8);
#4868=VECTOR('',#19548,0.8);
#4869=VECTOR('',#19553,1.);
#4870=VECTOR('',#19554,1.);
#4871=VECTOR('',#19557,1.);
#4872=VECTOR('',#19560,1.);
#4873=VECTOR('',#19563,1.);
#4874=VECTOR('',#19566,1.);
#4875=VECTOR('',#19569,1.);
#4876=VECTOR('',#19572,1.);
#4877=VECTOR('',#19575,1.);
#4878=VECTOR('',#19578,1.);
#4879=VECTOR('',#19581,1.);
#4880=VECTOR('',#19584,1.);
#4881=VECTOR('',#19587,1.);
#4882=VECTOR('',#19590,1.);
#4883=VECTOR('',#19593,1.);
#4884=VECTOR('',#19596,1.);
#4885=VECTOR('',#19599,1.);
#4886=VECTOR('',#19602,1.);
#4887=VECTOR('',#19605,1.);
#4888=VECTOR('',#19608,1.);
#4889=VECTOR('',#19611,1.);
#4890=VECTOR('',#19614,1.);
#4891=VECTOR('',#19617,1.);
#4892=VECTOR('',#19620,1.);
#4893=VECTOR('',#19623,1.);
#4894=VECTOR('',#19626,1.);
#4895=VECTOR('',#19629,1.);
#4896=VECTOR('',#19632,1.);
#4897=VECTOR('',#19635,1.);
#4898=VECTOR('',#19638,1.);
#4899=VECTOR('',#19641,1.);
#4900=VECTOR('',#19644,1.);
#4901=VECTOR('',#19647,1.);
#4902=VECTOR('',#19650,1.);
#4903=VECTOR('',#19653,1.);
#4904=VECTOR('',#19656,1.);
#4905=VECTOR('',#19659,1.);
#4906=VECTOR('',#19662,1.);
#4907=VECTOR('',#19665,1.);
#4908=VECTOR('',#19668,1.);
#4909=VECTOR('',#19685,1.);
#4910=VECTOR('',#19692,0.165);
#4911=VECTOR('',#19705,0.8);
#4912=VECTOR('',#19708,0.6);
#4913=VECTOR('',#19719,0.605);
#4914=VECTOR('',#19726,0.8);
#4915=VECTOR('',#19739,0.605);
#4916=VECTOR('',#19746,0.8);
#4917=VECTOR('',#19759,0.15);
#4918=VECTOR('',#19772,0.15);
#4919=VECTOR('',#19785,0.225);
#4920=VECTOR('',#19792,0.8);
#4921=VECTOR('',#19803,1.);
#4922=VECTOR('',#19810,0.21);
#4923=VECTOR('',#19815,1.);
#4924=VECTOR('',#19820,1.005);
#4925=VECTOR('',#19827,1.5);
#4926=VECTOR('',#19838,1.);
#4927=VECTOR('',#19845,0.21);
#4928=VECTOR('',#19850,1.);
#4929=VECTOR('',#19855,1.005);
#4930=VECTOR('',#19862,1.5);
#4931=VECTOR('',#19875,3.6);
#4932=VECTOR('',#19882,4.);
#4933=VECTOR('',#19895,1.005);
#4934=VECTOR('',#19902,4.);
#4935=VECTOR('',#19915,1.005);
#4936=VECTOR('',#19922,4.);
#4937=VECTOR('',#19933,1.);
#4938=VECTOR('',#19940,0.21);
#4939=VECTOR('',#19945,1.);
#4940=VECTOR('',#19950,1.005);
#4941=VECTOR('',#19957,1.8);
#4942=VECTOR('',#19968,1.);
#4943=VECTOR('',#19975,0.21);
#4944=VECTOR('',#19980,1.);
#4945=VECTOR('',#19985,1.005);
#4946=VECTOR('',#19992,1.8);
#4947=VECTOR('',#20003,0.125);
#4948=VECTOR('',#20006,0.125);
#4949=VECTOR('',#20011,1.);
#4950=VECTOR('',#20012,1.);
#4951=VECTOR('',#20017,0.125);
#4952=VECTOR('',#20020,0.125);
#4953=VECTOR('',#20025,0.6);
#4954=VECTOR('',#20026,0.6);
#4955=VECTOR('',#20199,1.4);
#4956=VECTOR('',#20370,1.4);
#4957=VECTOR('',#20375,1.);
#4958=VECTOR('',#20376,1.);
#4959=VECTOR('',#20379,1.);
#4960=VECTOR('',#20382,1.);
#4961=VECTOR('',#20385,1.);
#4962=VECTOR('',#20388,1.);
#4963=VECTOR('',#20391,1.);
#4964=VECTOR('',#20394,1.);
#4965=VECTOR('',#20397,1.);
#4966=VECTOR('',#20400,1.);
#4967=VECTOR('',#20403,1.);
#4968=VECTOR('',#20406,1.);
#4969=VECTOR('',#20409,1.);
#4970=VECTOR('',#20412,1.);
#4971=VECTOR('',#20415,1.);
#4972=VECTOR('',#20418,1.);
#4973=VECTOR('',#20421,1.);
#4974=VECTOR('',#20424,1.);
#4975=VECTOR('',#20427,1.);
#4976=VECTOR('',#20430,1.);
#4977=VECTOR('',#20433,1.);
#4978=VECTOR('',#20436,1.);
#4979=VECTOR('',#20439,1.);
#4980=VECTOR('',#20442,1.);
#4981=VECTOR('',#20445,1.);
#4982=VECTOR('',#20448,1.);
#4983=VECTOR('',#20451,1.);
#4984=VECTOR('',#20454,1.);
#4985=VECTOR('',#20457,1.);
#4986=VECTOR('',#20460,1.);
#4987=VECTOR('',#20463,1.);
#4988=VECTOR('',#20466,1.);
#4989=VECTOR('',#20469,1.);
#4990=VECTOR('',#20472,1.);
#4991=VECTOR('',#20475,1.);
#4992=VECTOR('',#20478,1.);
#4993=VECTOR('',#20481,1.);
#4994=VECTOR('',#20484,1.);
#4995=VECTOR('',#20487,1.);
#4996=VECTOR('',#20490,1.);
#4997=VECTOR('',#20493,1.);
#4998=VECTOR('',#20496,1.);
#4999=VECTOR('',#20499,1.);
#5000=VECTOR('',#20502,1.);
#5001=VECTOR('',#20505,1.);
#5002=VECTOR('',#20508,1.);
#5003=VECTOR('',#20511,1.);
#5004=VECTOR('',#20514,1.);
#5005=VECTOR('',#20517,1.);
#5006=VECTOR('',#20520,1.);
#5007=VECTOR('',#20523,1.);
#5008=VECTOR('',#20526,1.);
#5009=VECTOR('',#20529,1.);
#5010=VECTOR('',#20532,1.);
#5011=VECTOR('',#20535,1.);
#5012=VECTOR('',#20538,1.);
#5013=VECTOR('',#20541,1.);
#5014=VECTOR('',#20544,1.);
#5015=VECTOR('',#20547,1.);
#5016=VECTOR('',#20550,1.);
#5017=VECTOR('',#20553,1.);
#5018=VECTOR('',#20556,1.);
#5019=VECTOR('',#20559,1.);
#5020=VECTOR('',#20562,1.);
#5021=VECTOR('',#20565,1.);
#5022=VECTOR('',#20568,1.);
#5023=VECTOR('',#20571,1.);
#5024=VECTOR('',#20574,1.);
#5025=VECTOR('',#20577,1.);
#5026=VECTOR('',#20580,1.);
#5027=VECTOR('',#20583,1.);
#5028=VECTOR('',#20586,1.);
#5029=VECTOR('',#20589,1.);
#5030=VECTOR('',#20592,1.);
#5031=VECTOR('',#20595,1.);
#5032=VECTOR('',#20598,1.);
#5033=VECTOR('',#20601,1.);
#5034=VECTOR('',#20604,1.);
#5035=VECTOR('',#20607,1.);
#5036=VECTOR('',#20610,1.);
#5037=VECTOR('',#20623,0.325);
#5038=VECTOR('',#20628,0.35);
#5039=VECTOR('',#20633,0.335);
#5040=VECTOR('',#20642,0.21);
#5041=VECTOR('',#20647,0.2);
#5042=VECTOR('',#20652,0.18);
#5043=VECTOR('',#20657,1.);
#5044=VECTOR('',#20658,1.);
#5045=VECTOR('',#20659,1.);
#5046=VECTOR('',#20660,1.);
#5047=VECTOR('',#20663,1.);
#5048=VECTOR('',#20664,1.);
#5049=VECTOR('',#20665,1.);
#5050=VECTOR('',#20668,1.);
#5051=VECTOR('',#20669,1.);
#5052=VECTOR('',#20670,1.);
#5053=VECTOR('',#20673,1.);
#5054=VECTOR('',#20674,1.);
#5055=VECTOR('',#20675,1.);
#5056=VECTOR('',#20678,1.);
#5057=VECTOR('',#20679,1.);
#5058=VECTOR('',#20680,1.);
#5059=VECTOR('',#20683,1.);
#5060=VECTOR('',#20684,1.);
#5061=VECTOR('',#20851,1.);
#5062=VECTOR('',#20852,1.);
#5063=VECTOR('',#20853,1.);
#5064=VECTOR('',#20854,1.);
#5065=VECTOR('',#20857,1.);
#5066=VECTOR('',#20858,1.);
#5067=VECTOR('',#20859,1.);
#5068=VECTOR('',#20862,1.);
#5069=VECTOR('',#20863,1.);
#5070=VECTOR('',#20864,1.);
#5071=VECTOR('',#20867,1.);
#5072=VECTOR('',#20868,1.);
#5073=VECTOR('',#20869,1.);
#5074=VECTOR('',#20872,1.);
#5075=VECTOR('',#20873,1.);
#5076=VECTOR('',#20874,1.);
#5077=VECTOR('',#20877,1.);
#5078=VECTOR('',#20878,1.);
#5079=VECTOR('',#20889,0.235);
#5080=VECTOR('',#20894,0.25);
#5081=VECTOR('',#20899,0.2125);
#5082=CIRCLE('',#14566,0.165);
#5083=CIRCLE('',#14567,0.165);
#5084=CIRCLE('',#14570,0.165);
#5085=CIRCLE('',#14571,0.165);
#5086=CIRCLE('',#14574,0.210000000000001);
#5087=CIRCLE('',#14575,0.210000000000001);
#5088=CIRCLE('',#14578,0.210000000000001);
#5089=CIRCLE('',#14579,0.210000000000001);
#5090=CIRCLE('',#14582,0.21);
#5091=CIRCLE('',#14583,0.21);
#5092=CIRCLE('',#14586,0.21);
#5093=CIRCLE('',#14587,0.21);
#5094=CIRCLE('',#14590,0.210000000000001);
#5095=CIRCLE('',#14591,0.210000000000001);
#5096=CIRCLE('',#14594,0.210000000000001);
#5097=CIRCLE('',#14595,0.210000000000001);
#5098=CIRCLE('',#14598,0.21);
#5099=CIRCLE('',#14599,0.21);
#5100=CIRCLE('',#14602,0.21);
#5101=CIRCLE('',#14603,0.21);
#5102=CIRCLE('',#14606,0.225);
#5103=CIRCLE('',#14607,0.225);
#5104=CIRCLE('',#14609,0.225);
#5105=CIRCLE('',#14610,0.225);
#5106=CIRCLE('',#14612,0.225);
#5107=CIRCLE('',#14613,0.225);
#5108=CIRCLE('',#14614,0.225);
#5109=CIRCLE('',#14615,0.225);
#5110=CIRCLE('',#14616,0.225);
#5111=CIRCLE('',#14617,0.225);
#5112=CIRCLE('',#14621,0.225);
#5113=CIRCLE('',#14623,0.225);
#5114=CIRCLE('',#14627,0.225);
#5115=CIRCLE('',#14628,0.225);
#5116=CIRCLE('',#14629,0.225);
#5117=CIRCLE('',#14631,0.225);
#5118=CIRCLE('',#14635,0.225);
#5119=CIRCLE('',#14636,0.225);
#5120=CIRCLE('',#14637,0.225);
#5121=CIRCLE('',#14639,0.225);
#5122=CIRCLE('',#14643,0.165);
#5123=CIRCLE('',#14644,0.165);
#5124=CIRCLE('',#14647,0.165);
#5125=CIRCLE('',#14648,0.165);
#5126=CIRCLE('',#14651,0.165);
#5127=CIRCLE('',#14652,0.165);
#5128=CIRCLE('',#14655,0.165);
#5129=CIRCLE('',#14656,0.165);
#5130=CIRCLE('',#14679,0.165);
#5131=CIRCLE('',#14680,0.165);
#5132=CIRCLE('',#14682,0.165);
#5133=CIRCLE('',#14683,0.165);
#5134=CIRCLE('',#14685,0.165);
#5135=CIRCLE('',#14686,0.165);
#5136=CIRCLE('',#14688,0.165);
#5137=CIRCLE('',#14689,0.165);
#5138=CIRCLE('',#14691,1.5);
#5139=CIRCLE('',#14692,1.5);
#5140=CIRCLE('',#14694,0.225);
#5141=CIRCLE('',#14695,0.225);
#5142=CIRCLE('',#14697,0.225);
#5143=CIRCLE('',#14698,0.225);
#5144=CIRCLE('',#14700,0.225);
#5145=CIRCLE('',#14701,0.225);
#5146=CIRCLE('',#14703,0.225);
#5147=CIRCLE('',#14704,0.225);
#5148=CIRCLE('',#14717,1.1);
#5149=CIRCLE('',#14718,1.1);
#5150=CIRCLE('',#14720,1.49);
#5151=CIRCLE('',#14721,1.49);
#5152=CIRCLE('',#14726,0.225);
#5153=CIRCLE('',#14727,0.225);
#5154=CIRCLE('',#14729,0.225);
#5155=CIRCLE('',#14730,0.225);
#5156=CIRCLE('',#14732,0.225);
#5157=CIRCLE('',#14733,0.225);
#5158=CIRCLE('',#14735,0.225);
#5159=CIRCLE('',#14736,0.225);
#5160=CIRCLE('',#14738,2.1);
#5161=CIRCLE('',#14739,2.1);
#5162=CIRCLE('',#14740,2.1);
#5163=CIRCLE('',#14741,2.1);
#5164=CIRCLE('',#14742,1.1);
#5165=CIRCLE('',#14744,2.1);
#5166=CIRCLE('',#14746,2.1);
#5167=CIRCLE('',#14748,2.1);
#5168=CIRCLE('',#14750,2.1);
#5169=CIRCLE('',#14752,1.49);
#5170=CIRCLE('',#14753,1.49);
#5171=CIRCLE('',#14755,1.1);
#5172=CIRCLE('',#14760,0.225);
#5173=CIRCLE('',#14761,0.225);
#5174=CIRCLE('',#14763,0.225);
#5175=CIRCLE('',#14764,0.225);
#5176=CIRCLE('',#14766,0.225);
#5177=CIRCLE('',#14767,0.225);
#5178=CIRCLE('',#14769,0.225);
#5179=CIRCLE('',#14770,0.225);
#5180=CIRCLE('',#14772,2.1);
#5181=CIRCLE('',#14773,2.1);
#5182=CIRCLE('',#14774,2.1);
#5183=CIRCLE('',#14775,2.1);
#5184=CIRCLE('',#14776,1.49);
#5185=CIRCLE('',#14778,2.1);
#5186=CIRCLE('',#14780,2.1);
#5187=CIRCLE('',#14782,2.1);
#5188=CIRCLE('',#14784,2.1);
#5189=CIRCLE('',#14786,1.49);
#5190=CIRCLE('',#14788,1.1);
#5191=CIRCLE('',#14790,1.1);
#5192=CIRCLE('',#14794,2.21);
#5193=CIRCLE('',#14795,2.21);
#5194=CIRCLE('',#14797,2.21);
#5195=CIRCLE('',#14798,2.21);
#5196=CIRCLE('',#14800,2.21);
#5197=CIRCLE('',#14801,1.6);
#5198=CIRCLE('',#14802,0.164999999999999);
#5199=CIRCLE('',#14803,0.164999999999999);
#5200=CIRCLE('',#14804,0.165);
#5201=CIRCLE('',#14805,0.165);
#5202=CIRCLE('',#14807,2.21);
#5203=CIRCLE('',#14813,0.165);
#5204=CIRCLE('',#14815,0.165);
#5205=CIRCLE('',#14817,0.164999999999999);
#5206=CIRCLE('',#14819,0.164999999999999);
#5207=CIRCLE('',#14821,1.6);
#5208=CIRCLE('',#14823,0.225);
#5209=CIRCLE('',#14824,0.225);
#5210=CIRCLE('',#14826,0.225);
#5211=CIRCLE('',#14827,0.225);
#5212=CIRCLE('',#14829,0.225);
#5213=CIRCLE('',#14830,0.225);
#5214=CIRCLE('',#14832,0.225);
#5215=CIRCLE('',#14833,0.225);
#5216=CIRCLE('',#14844,0.165);
#5217=CIRCLE('',#14845,0.165);
#5218=CIRCLE('',#14847,0.4);
#5219=CIRCLE('',#14848,0.4);
#5220=CIRCLE('',#14853,0.165);
#5221=CIRCLE('',#14854,0.165);
#5222=CIRCLE('',#14856,0.4);
#5223=CIRCLE('',#14857,0.4);
#5224=CIRCLE('',#14862,0.164999999999999);
#5225=CIRCLE('',#14863,0.164999999999999);
#5226=CIRCLE('',#14865,0.4);
#5227=CIRCLE('',#14866,0.4);
#5228=CIRCLE('',#14871,0.164999999999999);
#5229=CIRCLE('',#14872,0.164999999999999);
#5230=CIRCLE('',#14874,0.4);
#5231=CIRCLE('',#14875,0.4);
#5232=CIRCLE('',#14880,1.2);
#5233=CIRCLE('',#14881,1.2);
#5234=CIRCLE('',#14883,1.59);
#5235=CIRCLE('',#14884,1.59);
#5236=CIRCLE('',#14889,0.225);
#5237=CIRCLE('',#14890,0.225);
#5238=CIRCLE('',#14892,0.225);
#5239=CIRCLE('',#14893,0.225);
#5240=CIRCLE('',#14895,0.225);
#5241=CIRCLE('',#14896,0.225);
#5242=CIRCLE('',#14898,0.225);
#5243=CIRCLE('',#14899,0.225);
#5244=CIRCLE('',#14901,2.2);
#5245=CIRCLE('',#14902,2.2);
#5246=CIRCLE('',#14903,2.2);
#5247=CIRCLE('',#14904,2.2);
#5248=CIRCLE('',#14905,1.2);
#5249=CIRCLE('',#14907,2.2);
#5250=CIRCLE('',#14909,2.2);
#5251=CIRCLE('',#14911,2.2);
#5252=CIRCLE('',#14913,2.2);
#5253=CIRCLE('',#14915,1.59);
#5254=CIRCLE('',#14916,1.59);
#5255=CIRCLE('',#14918,1.2);
#5256=CIRCLE('',#14923,0.375);
#5257=CIRCLE('',#14924,0.375);
#5258=CIRCLE('',#14926,2.2);
#5259=CIRCLE('',#14927,0.225);
#5260=CIRCLE('',#14928,2.2);
#5261=CIRCLE('',#14930,2.2);
#5262=CIRCLE('',#14931,0.375);
#5263=CIRCLE('',#14932,2.2);
#5264=CIRCLE('',#14933,0.225);
#5265=CIRCLE('',#14935,0.375);
#5266=CIRCLE('',#14937,2.2);
#5267=CIRCLE('',#14938,0.375);
#5268=CIRCLE('',#14939,2.2);
#5269=CIRCLE('',#14940,0.225);
#5270=CIRCLE('',#14942,0.375);
#5271=CIRCLE('',#14944,2.2);
#5272=CIRCLE('',#14945,0.375);
#5273=CIRCLE('',#14946,2.2);
#5274=CIRCLE('',#14947,0.225);
#5275=CIRCLE('',#14949,0.375);
#5276=CIRCLE('',#14951,0.225);
#5277=CIRCLE('',#14953,0.225);
#5278=CIRCLE('',#14955,0.225);
#5279=CIRCLE('',#14957,2.2);
#5280=CIRCLE('',#14958,2.2);
#5281=CIRCLE('',#14960,2.2);
#5282=CIRCLE('',#14961,2.2);
#5283=CIRCLE('',#14962,2.2);
#5284=CIRCLE('',#14963,1.2);
#5285=CIRCLE('',#14965,0.225);
#5286=CIRCLE('',#14966,2.2);
#5287=CIRCLE('',#14967,2.2);
#5288=CIRCLE('',#14968,2.2);
#5289=CIRCLE('',#14969,1.2);
#5290=CIRCLE('',#14979,0.736619772367581);
#5291=CIRCLE('',#14980,1.37323954473516);
#5292=CIRCLE('',#14981,0.636619772367581);
#5293=CIRCLE('',#14982,1.27323954473516);
#5294=CIRCLE('',#14984,0.636619772367581);
#5295=CIRCLE('',#14986,1.27323954473516);
#5296=CIRCLE('',#14988,1.37323954473516);
#5297=CIRCLE('',#14992,0.736619772367581);
#5298=CIRCLE('',#14996,0.475);
#5299=CIRCLE('',#14997,0.475);
#5300=CIRCLE('',#14999,0.275);
#5301=CIRCLE('',#15001,0.275);
#5302=CIRCLE('',#15003,0.475);
#5303=CIRCLE('',#15004,0.475);
#5304=CIRCLE('',#15006,0.275);
#5305=CIRCLE('',#15008,0.275);
#5306=CIRCLE('',#15010,0.475);
#5307=CIRCLE('',#15011,0.475);
#5308=CIRCLE('',#15013,0.275);
#5309=CIRCLE('',#15015,0.275);
#5310=CIRCLE('',#15017,0.475);
#5311=CIRCLE('',#15018,0.475);
#5312=CIRCLE('',#15020,0.275);
#5313=CIRCLE('',#15022,0.275);
#5314=CIRCLE('',#15024,0.34);
#5315=CIRCLE('',#15025,0.34);
#5316=CIRCLE('',#15028,0.34);
#5317=CIRCLE('',#15029,0.34);
#5318=CIRCLE('',#15039,0.425);
#5319=CIRCLE('',#15040,0.425);
#5320=CIRCLE('',#15042,0.645);
#5321=CIRCLE('',#15043,0.645);
#5322=CIRCLE('',#15048,0.425000000000001);
#5323=CIRCLE('',#15049,0.425000000000001);
#5324=CIRCLE('',#15051,0.645);
#5325=CIRCLE('',#15052,0.645);
#5326=CIRCLE('',#15057,0.475);
#5327=CIRCLE('',#15058,0.475);
#5328=CIRCLE('',#15060,0.275);
#5329=CIRCLE('',#15062,0.275);
#5330=CIRCLE('',#15064,0.475);
#5331=CIRCLE('',#15065,0.475);
#5332=CIRCLE('',#15067,0.275);
#5333=CIRCLE('',#15069,0.275);
#5334=CIRCLE('',#15071,0.475);
#5335=CIRCLE('',#15072,0.475);
#5336=CIRCLE('',#15074,0.275);
#5337=CIRCLE('',#15076,0.275);
#5338=CIRCLE('',#15078,0.475);
#5339=CIRCLE('',#15079,0.475);
#5340=CIRCLE('',#15081,0.275);
#5341=CIRCLE('',#15083,0.275);
#5342=CIRCLE('',#15085,0.34);
#5343=CIRCLE('',#15086,0.34);
#5344=CIRCLE('',#15089,0.34);
#5345=CIRCLE('',#15090,0.34);
#5346=CIRCLE('',#15100,0.425);
#5347=CIRCLE('',#15101,0.425);
#5348=CIRCLE('',#15103,0.645);
#5349=CIRCLE('',#15104,0.645);
#5350=CIRCLE('',#15109,0.425000000000001);
#5351=CIRCLE('',#15110,0.425000000000001);
#5352=CIRCLE('',#15112,0.645);
#5353=CIRCLE('',#15113,0.645);
#5354=CIRCLE('',#15118,0.4);
#5355=CIRCLE('',#15119,0.4);
#5356=CIRCLE('',#15121,0.225);
#5357=CIRCLE('',#15123,0.225);
#5358=CIRCLE('',#15125,0.4);
#5359=CIRCLE('',#15126,0.4);
#5360=CIRCLE('',#15128,0.225);
#5361=CIRCLE('',#15130,0.225);
#5362=CIRCLE('',#15146,0.165);
#5363=CIRCLE('',#15147,0.165);
#5364=CIRCLE('',#15149,0.165);
#5365=CIRCLE('',#15150,0.165);
#5366=CIRCLE('',#15159,0.164999999999999);
#5367=CIRCLE('',#15160,0.164999999999999);
#5368=CIRCLE('',#15162,0.164999999999999);
#5369=CIRCLE('',#15163,0.164999999999999);
#5370=CIRCLE('',#15172,0.225);
#5371=CIRCLE('',#15173,0.225);
#5372=CIRCLE('',#15175,0.225);
#5373=CIRCLE('',#15176,0.225);
#5374=CIRCLE('',#15178,0.225);
#5375=CIRCLE('',#15179,0.225);
#5376=CIRCLE('',#15181,0.225);
#5377=CIRCLE('',#15182,0.225);
#5378=CIRCLE('',#15192,0.976185);
#5379=CIRCLE('',#15193,0.976185);
#5380=CIRCLE('',#15194,0.247676);
#5381=CIRCLE('',#15195,0.976185);
#5382=CIRCLE('',#15196,0.976185);
#5383=CIRCLE('',#15198,0.976185);
#5384=CIRCLE('',#15200,0.5);
#5385=CIRCLE('',#15201,0.5);
#5386=CIRCLE('',#15203,0.56);
#5387=CIRCLE('',#15206,0.976185);
#5388=CIRCLE('',#15208,0.56);
#5389=CIRCLE('',#15212,1.023815);
#5390=CIRCLE('',#15213,1.023815);
#5391=CIRCLE('',#15214,0.247676);
#5392=CIRCLE('',#15215,1.023815);
#5393=CIRCLE('',#15216,1.023815);
#5394=CIRCLE('',#15218,1.023815);
#5395=CIRCLE('',#15220,1.44);
#5396=CIRCLE('',#15221,1.023815);
#5397=CIRCLE('',#15223,1.5);
#5398=CIRCLE('',#15225,1.5);
#5399=CIRCLE('',#15227,1.44);
#5400=CIRCLE('',#15232,0.23815);
#5401=CIRCLE('',#15234,0.23815);
#5402=CIRCLE('',#15236,0.23815);
#5403=CIRCLE('',#15238,0.23815);
#5404=CIRCLE('',#15240,0.23815);
#5405=CIRCLE('',#15242,0.23815);
#5406=CIRCLE('',#15244,0.23815);
#5407=CIRCLE('',#15246,0.23815);
#5408=CIRCLE('',#15249,0.243053047864041);
#5409=CIRCLE('',#15250,0.243053047864041);
#5410=CIRCLE('',#15252,1.019052);
#5411=CIRCLE('',#15253,1.019052);
#5412=CIRCLE('',#15254,1.019052);
#5413=CIRCLE('',#15255,1.019052);
#5414=CIRCLE('',#15256,1.019052);
#5415=CIRCLE('',#15257,1.019052);
#5416=CIRCLE('',#15258,1.019052);
#5417=CIRCLE('',#15259,1.019052);
#5418=CIRCLE('',#15260,1.019052);
#5419=CIRCLE('',#15262,0.980948);
#5420=CIRCLE('',#15263,0.243053047864041);
#5421=CIRCLE('',#15265,0.243053047864041);
#5422=CIRCLE('',#15267,0.980948);
#5423=CIRCLE('',#15268,0.243053047864041);
#5424=CIRCLE('',#15270,0.243053047864041);
#5425=CIRCLE('',#15272,0.980948);
#5426=CIRCLE('',#15273,0.243053047864041);
#5427=CIRCLE('',#15275,0.243053047864041);
#5428=CIRCLE('',#15277,0.980948);
#5429=CIRCLE('',#15278,0.243053047864041);
#5430=CIRCLE('',#15280,0.243053047864041);
#5431=CIRCLE('',#15282,0.980948);
#5432=CIRCLE('',#15283,0.243053047864041);
#5433=CIRCLE('',#15285,0.243053047864041);
#5434=CIRCLE('',#15287,0.980948);
#5435=CIRCLE('',#15288,0.243053047864041);
#5436=CIRCLE('',#15290,0.243053047864041);
#5437=CIRCLE('',#15292,0.980948);
#5438=CIRCLE('',#15293,0.980948);
#5439=CIRCLE('',#15294,0.980948);
#5440=CIRCLE('',#15296,0.243053047864041);
#5441=CIRCLE('',#15298,0.243053047864041);
#5442=CIRCLE('',#15303,1.013815);
#5443=CIRCLE('',#15304,0.991185);
#5444=CIRCLE('',#15306,1.013815);
#5445=CIRCLE('',#15308,0.991185);
#5446=CIRCLE('',#15311,1.013815);
#5447=CIRCLE('',#15312,0.991185);
#5448=CIRCLE('',#15314,1.013815);
#5449=CIRCLE('',#15316,0.991185);
#5450=CIRCLE('',#15333,0.2);
#5451=CIRCLE('',#15334,0.16);
#5452=CIRCLE('',#15336,0.2);
#5453=CIRCLE('',#15339,0.3);
#5454=CIRCLE('',#15341,0.35);
#5455=CIRCLE('',#15343,0.35);
#5456=CIRCLE('',#15345,0.32);
#5457=CIRCLE('',#15347,0.22);
#5458=CIRCLE('',#15349,0.1954);
#5459=CIRCLE('',#15351,0.1954);
#5460=CIRCLE('',#15356,1.070235);
#5461=CIRCLE('',#15357,1.070235);
#5462=CIRCLE('',#15358,0.309556);
#5463=CIRCLE('',#15359,1.070235);
#5464=CIRCLE('',#15360,1.070235);
#5465=CIRCLE('',#15362,1.070235);
#5466=CIRCLE('',#15364,0.6);
#5467=CIRCLE('',#15365,0.6);
#5468=CIRCLE('',#15367,0.66);
#5469=CIRCLE('',#15370,1.070235);
#5470=CIRCLE('',#15372,0.66);
#5471=CIRCLE('',#15376,1.129765);
#5472=CIRCLE('',#15377,1.129765);
#5473=CIRCLE('',#15378,0.309556);
#5474=CIRCLE('',#15379,1.129765);
#5475=CIRCLE('',#15380,1.129765);
#5476=CIRCLE('',#15382,1.129765);
#5477=CIRCLE('',#15384,1.54);
#5478=CIRCLE('',#15385,1.129765);
#5479=CIRCLE('',#15387,1.6);
#5480=CIRCLE('',#15389,1.6);
#5481=CIRCLE('',#15391,1.54);
#5482=CIRCLE('',#15396,0.29765);
#5483=CIRCLE('',#15398,0.29765);
#5484=CIRCLE('',#15400,0.29765);
#5485=CIRCLE('',#15402,0.29765);
#5486=CIRCLE('',#15404,0.29765);
#5487=CIRCLE('',#15406,0.29765);
#5488=CIRCLE('',#15408,0.29765);
#5489=CIRCLE('',#15411,0.303778037777585);
#5490=CIRCLE('',#15412,0.303778037777585);
#5491=CIRCLE('',#15414,1.123812);
#5492=CIRCLE('',#15415,1.123812);
#5493=CIRCLE('',#15416,1.123812);
#5494=CIRCLE('',#15417,1.123812);
#5495=CIRCLE('',#15418,1.123812);
#5496=CIRCLE('',#15419,1.123812);
#5497=CIRCLE('',#15420,1.123812);
#5498=CIRCLE('',#15421,1.123812);
#5499=CIRCLE('',#15422,1.123812);
#5500=CIRCLE('',#15424,1.076188);
#5501=CIRCLE('',#15425,0.303778037777585);
#5502=CIRCLE('',#15427,0.303778037777585);
#5503=CIRCLE('',#15429,1.076188);
#5504=CIRCLE('',#15430,0.303778037777585);
#5505=CIRCLE('',#15432,0.303778037777585);
#5506=CIRCLE('',#15434,1.076188);
#5507=CIRCLE('',#15435,1.076188);
#5508=CIRCLE('',#15436,0.303778037777585);
#5509=CIRCLE('',#15438,0.303778037777585);
#5510=CIRCLE('',#15440,1.076188);
#5511=CIRCLE('',#15441,0.303778037777585);
#5512=CIRCLE('',#15443,0.303778037777585);
#5513=CIRCLE('',#15445,1.076188);
#5514=CIRCLE('',#15446,0.303778037777585);
#5515=CIRCLE('',#15448,0.303778037777585);
#5516=CIRCLE('',#15450,1.076188);
#5517=CIRCLE('',#15451,1.076188);
#5518=CIRCLE('',#15452,1.076188);
#5519=CIRCLE('',#15454,0.303778037777585);
#5520=CIRCLE('',#15456,0.303778037777585);
#5521=CIRCLE('',#15461,1.119765);
#5522=CIRCLE('',#15462,1.085235);
#5523=CIRCLE('',#15464,1.119765);
#5524=CIRCLE('',#15466,1.085235);
#5525=CIRCLE('',#15469,1.119765);
#5526=CIRCLE('',#15470,1.085235);
#5527=CIRCLE('',#15472,1.119765);
#5528=CIRCLE('',#15474,1.085235);
#5529=CIRCLE('',#15483,0.375);
#5530=CIRCLE('',#15485,0.425);
#5531=CIRCLE('',#15487,0.425);
#5532=CIRCLE('',#15489,0.395);
#5533=CIRCLE('',#15491,0.27);
#5534=CIRCLE('',#15493,0.24505);
#5535=CIRCLE('',#15495,0.24505);
#5536=CIRCLE('',#15497,0.2);
#5537=CIRCLE('',#15510,2.05);
#5538=CIRCLE('',#15511,2.05);
#5539=CIRCLE('',#15513,2.05);
#5540=CIRCLE('',#15514,2.05);
#5541=CIRCLE('',#15516,2.35);
#5542=CIRCLE('',#15518,2.8);
#5543=CIRCLE('',#15520,2.8);
#5544=CIRCLE('',#15522,2.8);
#5545=CIRCLE('',#15525,2.8);
#5546=CIRCLE('',#15528,0.65);
#5547=CIRCLE('',#15529,0.65);
#5548=CIRCLE('',#15531,2.8);
#5549=CIRCLE('',#15532,2.8);
#5550=CIRCLE('',#15541,0.65);
#5551=CIRCLE('',#15543,0.65);
#5552=CIRCLE('',#15551,1.8);
#5553=CIRCLE('',#15552,1.8);
#5554=CIRCLE('',#15554,2.19089023002066);
#5555=CIRCLE('',#15556,2.35);
#5556=CIRCLE('',#15557,2.19089023002066);
#5557=CIRCLE('',#15562,1.65);
#5558=CIRCLE('',#15563,1.65);
#5559=CIRCLE('',#15569,1.);
#5560=CIRCLE('',#15571,1.75);
#5561=CIRCLE('',#15573,1.75);
#5562=CIRCLE('',#15575,1.);
#5563=CIRCLE('',#15581,0.42);
#5564=CIRCLE('',#15582,0.42);
#5565=CIRCLE('',#15584,0.8);
#5566=CIRCLE('',#15585,0.8);
#5567=CIRCLE('',#15598,0.3933);
#5568=CIRCLE('',#15600,0.6);
#5569=CIRCLE('',#15602,0.65);
#5570=CIRCLE('',#15604,0.65);
#5571=CIRCLE('',#15606,0.62);
#5572=CIRCLE('',#15608,0.42);
#5573=CIRCLE('',#15610,0.3933);
#5574=CIRCLE('',#15622,0.1954);
#5575=CIRCLE('',#15624,0.3);
#5576=CIRCLE('',#15626,0.35);
#5577=CIRCLE('',#15628,0.35);
#5578=CIRCLE('',#15630,0.32);
#5579=CIRCLE('',#15632,0.22);
#5580=CIRCLE('',#15634,0.1954);
#5581=CIRCLE('',#15639,0.165);
#5582=CIRCLE('',#15640,0.165);
#5583=CIRCLE('',#15643,0.7);
#5584=CIRCLE('',#15644,0.5);
#5585=CIRCLE('',#15646,0.7);
#5586=CIRCLE('',#15647,0.5);
#5587=CIRCLE('',#15650,0.5);
#5588=CIRCLE('',#15652,0.4);
#5589=CIRCLE('',#15653,0.4);
#5590=CIRCLE('',#15656,0.5);
#5591=CIRCLE('',#15661,0.505);
#5592=CIRCLE('',#15662,0.505);
#5593=CIRCLE('',#15664,0.405);
#5594=CIRCLE('',#15666,0.405);
#5595=CIRCLE('',#15668,0.7);
#5596=CIRCLE('',#15669,0.7);
#5597=CIRCLE('',#15674,0.505);
#5598=CIRCLE('',#15675,0.505);
#5599=CIRCLE('',#15677,0.7);
#5600=CIRCLE('',#15678,0.7);
#5601=CIRCLE('',#15683,0.15);
#5602=CIRCLE('',#15684,0.15);
#5603=CIRCLE('',#15689,0.15);
#5604=CIRCLE('',#15690,0.15);
#5605=CIRCLE('',#15695,0.225);
#5606=CIRCLE('',#15696,0.225);
#5607=CIRCLE('',#15698,0.6);
#5608=CIRCLE('',#15699,0.6);
#5609=CIRCLE('',#15704,0.5);
#5610=CIRCLE('',#15705,0.5);
#5611=CIRCLE('',#15710,0.21);
#5612=CIRCLE('',#15712,0.21);
#5613=CIRCLE('',#15713,0.21);
#5614=CIRCLE('',#15716,0.21);
#5615=CIRCLE('',#15718,0.21);
#5616=CIRCLE('',#15719,0.21);
#5617=CIRCLE('',#15722,0.505);
#5618=CIRCLE('',#15723,0.505);
#5619=CIRCLE('',#15725,1.);
#5620=CIRCLE('',#15726,1.);
#5621=CIRCLE('',#15733,0.65);
#5622=CIRCLE('',#15734,0.65);
#5623=CIRCLE('',#15738,0.4);
#5624=CIRCLE('',#15739,0.4);
#5625=CIRCLE('',#15742,0.8);
#5626=CIRCLE('',#15743,0.0555);
#5627=CIRCLE('',#15744,0.611219772367581);
#5628=CIRCLE('',#15745,0.0555);
#5629=CIRCLE('',#15746,0.611219772367581);
#5630=CIRCLE('',#15747,0.0555);
#5631=CIRCLE('',#15748,0.611219772367581);
#5632=CIRCLE('',#15749,0.0555);
#5633=CIRCLE('',#15750,0.611219772367581);
#5634=CIRCLE('',#15751,0.0555);
#5635=CIRCLE('',#15752,0.611219772367581);
#5636=CIRCLE('',#15753,0.0555);
#5637=CIRCLE('',#15754,0.611219772367581);
#5638=CIRCLE('',#15755,0.0555);
#5639=CIRCLE('',#15756,0.611219772367581);
#5640=CIRCLE('',#15757,0.0555);
#5641=CIRCLE('',#15758,0.611219772367581);
#5642=CIRCLE('',#15759,0.0555);
#5643=CIRCLE('',#15760,0.611219772367581);
#5644=CIRCLE('',#15761,0.0555);
#5645=CIRCLE('',#15762,0.611219772367581);
#5646=CIRCLE('',#15763,0.0555);
#5647=CIRCLE('',#15764,0.611219772367581);
#5648=CIRCLE('',#15765,0.0555);
#5649=CIRCLE('',#15766,0.611219772367581);
#5650=CIRCLE('',#15767,0.0555);
#5651=CIRCLE('',#15768,0.611219772367581);
#5652=CIRCLE('',#15769,0.0555);
#5653=CIRCLE('',#15770,0.611219772367581);
#5654=CIRCLE('',#15771,0.0555);
#5655=CIRCLE('',#15772,0.611219772367581);
#5656=CIRCLE('',#15773,0.0555);
#5657=CIRCLE('',#15774,0.611219772367581);
#5658=CIRCLE('',#15775,0.0555);
#5659=CIRCLE('',#15776,0.611219772367581);
#5660=CIRCLE('',#15777,0.0555);
#5661=CIRCLE('',#15778,0.611219772367581);
#5662=CIRCLE('',#15779,0.0555);
#5663=CIRCLE('',#15780,0.611219772367581);
#5664=CIRCLE('',#15781,0.0555);
#5665=CIRCLE('',#15782,0.611219772367581);
#5666=CIRCLE('',#15784,0.8);
#5667=CIRCLE('',#15787,0.8);
#5668=CIRCLE('',#15788,0.0555);
#5669=CIRCLE('',#15789,0.611219772367581);
#5670=CIRCLE('',#15790,0.0555);
#5671=CIRCLE('',#15791,0.611219772367581);
#5672=CIRCLE('',#15792,0.0555);
#5673=CIRCLE('',#15793,0.611219772367581);
#5674=CIRCLE('',#15794,0.0555);
#5675=CIRCLE('',#15795,0.611219772367581);
#5676=CIRCLE('',#15796,0.0555);
#5677=CIRCLE('',#15797,0.611219772367581);
#5678=CIRCLE('',#15798,0.0555);
#5679=CIRCLE('',#15799,0.611219772367581);
#5680=CIRCLE('',#15800,0.0555);
#5681=CIRCLE('',#15801,0.611219772367581);
#5682=CIRCLE('',#15802,0.0555);
#5683=CIRCLE('',#15803,0.611219772367581);
#5684=CIRCLE('',#15804,0.0555);
#5685=CIRCLE('',#15805,0.611219772367581);
#5686=CIRCLE('',#15806,0.0555);
#5687=CIRCLE('',#15807,0.611219772367581);
#5688=CIRCLE('',#15808,0.0555);
#5689=CIRCLE('',#15809,0.611219772367581);
#5690=CIRCLE('',#15810,0.0555);
#5691=CIRCLE('',#15811,0.611219772367581);
#5692=CIRCLE('',#15812,0.0555);
#5693=CIRCLE('',#15813,0.611219772367581);
#5694=CIRCLE('',#15814,0.0555);
#5695=CIRCLE('',#15815,0.611219772367581);
#5696=CIRCLE('',#15816,0.0555);
#5697=CIRCLE('',#15817,0.611219772367581);
#5698=CIRCLE('',#15818,0.0555);
#5699=CIRCLE('',#15819,0.611219772367581);
#5700=CIRCLE('',#15820,0.0555);
#5701=CIRCLE('',#15821,0.611219772367581);
#5702=CIRCLE('',#15822,0.0555);
#5703=CIRCLE('',#15823,0.611219772367581);
#5704=CIRCLE('',#15824,0.0555);
#5705=CIRCLE('',#15825,0.611219772367581);
#5706=CIRCLE('',#15826,0.0555);
#5707=CIRCLE('',#15827,0.611219772367581);
#5708=CIRCLE('',#15829,0.8);
#5709=CIRCLE('',#15874,1.);
#5710=CIRCLE('',#15875,0.8);
#5711=CIRCLE('',#15877,1.);
#5712=CIRCLE('',#15880,0.165);
#5713=CIRCLE('',#15881,0.165);
#5714=CIRCLE('',#15884,0.8);
#5715=CIRCLE('',#15885,0.6);
#5716=CIRCLE('',#15888,0.6);
#5717=CIRCLE('',#15892,0.605);
#5718=CIRCLE('',#15893,0.605);
#5719=CIRCLE('',#15895,0.8);
#5720=CIRCLE('',#15896,0.8);
#5721=CIRCLE('',#15901,0.605);
#5722=CIRCLE('',#15902,0.605);
#5723=CIRCLE('',#15904,0.8);
#5724=CIRCLE('',#15905,0.8);
#5725=CIRCLE('',#15910,0.15);
#5726=CIRCLE('',#15911,0.15);
#5727=CIRCLE('',#15916,0.15);
#5728=CIRCLE('',#15917,0.15);
#5729=CIRCLE('',#15922,0.225);
#5730=CIRCLE('',#15923,0.225);
#5731=CIRCLE('',#15925,0.8);
#5732=CIRCLE('',#15926,0.8);
#5733=CIRCLE('',#15931,0.21);
#5734=CIRCLE('',#15933,0.21);
#5735=CIRCLE('',#15934,0.21);
#5736=CIRCLE('',#15937,1.005);
#5737=CIRCLE('',#15938,1.005);
#5738=CIRCLE('',#15940,1.5);
#5739=CIRCLE('',#15941,1.5);
#5740=CIRCLE('',#15946,0.21);
#5741=CIRCLE('',#15948,0.21);
#5742=CIRCLE('',#15949,0.21);
#5743=CIRCLE('',#15952,1.005);
#5744=CIRCLE('',#15953,1.005);
#5745=CIRCLE('',#15955,1.5);
#5746=CIRCLE('',#15956,1.5);
#5747=CIRCLE('',#15961,3.6);
#5748=CIRCLE('',#15962,3.6);
#5749=CIRCLE('',#15964,4.);
#5750=CIRCLE('',#15965,4.);
#5751=CIRCLE('',#15970,1.005);
#5752=CIRCLE('',#15971,1.005);
#5753=CIRCLE('',#15973,4.);
#5754=CIRCLE('',#15974,4.);
#5755=CIRCLE('',#15979,1.005);
#5756=CIRCLE('',#15980,1.005);
#5757=CIRCLE('',#15982,4.);
#5758=CIRCLE('',#15983,4.);
#5759=CIRCLE('',#15988,0.21);
#5760=CIRCLE('',#15990,0.21);
#5761=CIRCLE('',#15991,0.21);
#5762=CIRCLE('',#15994,1.005);
#5763=CIRCLE('',#15995,1.005);
#5764=CIRCLE('',#15997,1.8);
#5765=CIRCLE('',#15998,1.8);
#5766=CIRCLE('',#16003,0.21);
#5767=CIRCLE('',#16005,0.21);
#5768=CIRCLE('',#16006,0.21);
#5769=CIRCLE('',#16009,1.005);
#5770=CIRCLE('',#16010,1.005);
#5771=CIRCLE('',#16012,1.8);
#5772=CIRCLE('',#16013,1.8);
#5773=CIRCLE('',#16020,1.);
#5774=CIRCLE('',#16021,1.);
#5775=CIRCLE('',#16025,0.6);
#5776=CIRCLE('',#16026,0.6);
#5777=CIRCLE('',#16029,1.4);
#5778=CIRCLE('',#16030,0.0555000000000001);
#5779=CIRCLE('',#16031,1.24783954473516);
#5780=CIRCLE('',#16032,0.0555000000000001);
#5781=CIRCLE('',#16033,1.24783954473516);
#5782=CIRCLE('',#16034,0.0555000000000001);
#5783=CIRCLE('',#16035,1.24783954473516);
#5784=CIRCLE('',#16036,0.0555000000000001);
#5785=CIRCLE('',#16037,1.24783954473516);
#5786=CIRCLE('',#16038,0.0555000000000001);
#5787=CIRCLE('',#16039,1.24783954473516);
#5788=CIRCLE('',#16040,0.0555000000000001);
#5789=CIRCLE('',#16041,1.24783954473516);
#5790=CIRCLE('',#16042,0.0555000000000001);
#5791=CIRCLE('',#16043,1.24783954473516);
#5792=CIRCLE('',#16044,0.0555000000000001);
#5793=CIRCLE('',#16045,1.24783954473516);
#5794=CIRCLE('',#16046,0.0555000000000001);
#5795=CIRCLE('',#16047,1.24783954473516);
#5796=CIRCLE('',#16048,0.0555000000000001);
#5797=CIRCLE('',#16049,1.24783954473516);
#5798=CIRCLE('',#16050,0.0555000000000001);
#5799=CIRCLE('',#16051,1.24783954473516);
#5800=CIRCLE('',#16052,0.0555000000000001);
#5801=CIRCLE('',#16053,1.24783954473516);
#5802=CIRCLE('',#16054,0.0555000000000001);
#5803=CIRCLE('',#16055,1.24783954473516);
#5804=CIRCLE('',#16056,0.0555000000000001);
#5805=CIRCLE('',#16057,1.24783954473516);
#5806=CIRCLE('',#16058,0.0555000000000001);
#5807=CIRCLE('',#16059,1.24783954473516);
#5808=CIRCLE('',#16060,0.0555000000000001);
#5809=CIRCLE('',#16061,1.24783954473516);
#5810=CIRCLE('',#16062,0.0555000000000001);
#5811=CIRCLE('',#16063,1.24783954473516);
#5812=CIRCLE('',#16064,0.0555000000000001);
#5813=CIRCLE('',#16065,1.24783954473516);
#5814=CIRCLE('',#16066,0.0555000000000001);
#5815=CIRCLE('',#16067,1.24783954473516);
#5816=CIRCLE('',#16068,0.0555000000000001);
#5817=CIRCLE('',#16069,1.24783954473516);
#5818=CIRCLE('',#16070,0.0555000000000001);
#5819=CIRCLE('',#16071,1.24783954473516);
#5820=CIRCLE('',#16072,0.0555000000000001);
#5821=CIRCLE('',#16073,1.24783954473516);
#5822=CIRCLE('',#16074,0.0555000000000001);
#5823=CIRCLE('',#16075,1.24783954473516);
#5824=CIRCLE('',#16076,0.0555000000000001);
#5825=CIRCLE('',#16077,1.24783954473516);
#5826=CIRCLE('',#16078,0.0555000000000001);
#5827=CIRCLE('',#16079,1.24783954473516);
#5828=CIRCLE('',#16080,0.0555000000000001);
#5829=CIRCLE('',#16081,1.24783954473516);
#5830=CIRCLE('',#16082,0.0555000000000001);
#5831=CIRCLE('',#16083,1.24783954473516);
#5832=CIRCLE('',#16084,0.0555000000000001);
#5833=CIRCLE('',#16085,1.24783954473516);
#5834=CIRCLE('',#16086,0.0555000000000001);
#5835=CIRCLE('',#16087,1.24783954473516);
#5836=CIRCLE('',#16088,0.0555000000000001);
#5837=CIRCLE('',#16089,1.24783954473516);
#5838=CIRCLE('',#16090,0.0555000000000001);
#5839=CIRCLE('',#16091,1.24783954473516);
#5840=CIRCLE('',#16092,0.0555000000000001);
#5841=CIRCLE('',#16093,1.24783954473516);
#5842=CIRCLE('',#16094,0.0555000000000001);
#5843=CIRCLE('',#16095,1.24783954473516);
#5844=CIRCLE('',#16096,0.0555000000000001);
#5845=CIRCLE('',#16097,1.24783954473516);
#5846=CIRCLE('',#16098,0.0555000000000001);
#5847=CIRCLE('',#16099,1.24783954473516);
#5848=CIRCLE('',#16100,0.0555000000000001);
#5849=CIRCLE('',#16101,1.24783954473516);
#5850=CIRCLE('',#16102,0.0555000000000001);
#5851=CIRCLE('',#16103,1.24783954473516);
#5852=CIRCLE('',#16104,0.0555000000000001);
#5853=CIRCLE('',#16105,1.24783954473516);
#5854=CIRCLE('',#16106,0.0555000000000001);
#5855=CIRCLE('',#16107,1.24783954473516);
#5856=CIRCLE('',#16108,0.0555000000000001);
#5857=CIRCLE('',#16109,1.24783954473516);
#5858=CIRCLE('',#16111,1.4);
#5859=CIRCLE('',#16114,1.4);
#5860=CIRCLE('',#16115,0.0555000000000001);
#5861=CIRCLE('',#16116,1.24783954473516);
#5862=CIRCLE('',#16117,0.0555000000000001);
#5863=CIRCLE('',#16118,1.24783954473516);
#5864=CIRCLE('',#16119,0.0555000000000001);
#5865=CIRCLE('',#16120,1.24783954473516);
#5866=CIRCLE('',#16121,0.0555000000000001);
#5867=CIRCLE('',#16122,1.24783954473516);
#5868=CIRCLE('',#16123,0.0555000000000001);
#5869=CIRCLE('',#16124,1.24783954473516);
#5870=CIRCLE('',#16125,0.0555000000000001);
#5871=CIRCLE('',#16126,1.24783954473516);
#5872=CIRCLE('',#16127,0.0555000000000001);
#5873=CIRCLE('',#16128,1.24783954473516);
#5874=CIRCLE('',#16129,0.0555000000000001);
#5875=CIRCLE('',#16130,1.24783954473516);
#5876=CIRCLE('',#16131,0.0555000000000001);
#5877=CIRCLE('',#16132,1.24783954473516);
#5878=CIRCLE('',#16133,0.0555000000000001);
#5879=CIRCLE('',#16134,1.24783954473516);
#5880=CIRCLE('',#16135,0.0555000000000001);
#5881=CIRCLE('',#16136,1.24783954473516);
#5882=CIRCLE('',#16137,0.0555000000000001);
#5883=CIRCLE('',#16138,1.24783954473516);
#5884=CIRCLE('',#16139,0.0555000000000001);
#5885=CIRCLE('',#16140,1.24783954473516);
#5886=CIRCLE('',#16141,0.0555000000000001);
#5887=CIRCLE('',#16142,1.24783954473516);
#5888=CIRCLE('',#16143,0.0555000000000001);
#5889=CIRCLE('',#16144,1.24783954473516);
#5890=CIRCLE('',#16145,0.0555000000000001);
#5891=CIRCLE('',#16146,1.24783954473516);
#5892=CIRCLE('',#16147,0.0555000000000001);
#5893=CIRCLE('',#16148,1.24783954473516);
#5894=CIRCLE('',#16149,0.0555000000000001);
#5895=CIRCLE('',#16150,1.24783954473516);
#5896=CIRCLE('',#16151,0.0555000000000001);
#5897=CIRCLE('',#16152,1.24783954473516);
#5898=CIRCLE('',#16153,0.0555000000000001);
#5899=CIRCLE('',#16154,1.24783954473516);
#5900=CIRCLE('',#16155,0.0555000000000001);
#5901=CIRCLE('',#16156,1.24783954473516);
#5902=CIRCLE('',#16157,0.0555000000000001);
#5903=CIRCLE('',#16158,1.24783954473516);
#5904=CIRCLE('',#16159,0.0555000000000001);
#5905=CIRCLE('',#16160,1.24783954473516);
#5906=CIRCLE('',#16161,0.0555000000000001);
#5907=CIRCLE('',#16162,1.24783954473516);
#5908=CIRCLE('',#16163,0.0555000000000001);
#5909=CIRCLE('',#16164,1.24783954473516);
#5910=CIRCLE('',#16165,0.0555000000000001);
#5911=CIRCLE('',#16166,1.24783954473516);
#5912=CIRCLE('',#16167,0.0555000000000001);
#5913=CIRCLE('',#16168,1.24783954473516);
#5914=CIRCLE('',#16169,0.0555000000000001);
#5915=CIRCLE('',#16170,1.24783954473516);
#5916=CIRCLE('',#16171,0.0555000000000001);
#5917=CIRCLE('',#16172,1.24783954473516);
#5918=CIRCLE('',#16173,0.0555000000000001);
#5919=CIRCLE('',#16174,1.24783954473516);
#5920=CIRCLE('',#16175,0.0555000000000001);
#5921=CIRCLE('',#16176,1.24783954473516);
#5922=CIRCLE('',#16177,0.0555000000000001);
#5923=CIRCLE('',#16178,1.24783954473516);
#5924=CIRCLE('',#16179,0.0555000000000001);
#5925=CIRCLE('',#16180,1.24783954473516);
#5926=CIRCLE('',#16181,0.0555000000000001);
#5927=CIRCLE('',#16182,1.24783954473516);
#5928=CIRCLE('',#16183,0.0555000000000001);
#5929=CIRCLE('',#16184,1.24783954473516);
#5930=CIRCLE('',#16185,0.0555000000000001);
#5931=CIRCLE('',#16186,1.24783954473516);
#5932=CIRCLE('',#16187,0.0555000000000001);
#5933=CIRCLE('',#16188,1.24783954473516);
#5934=CIRCLE('',#16189,0.0555000000000001);
#5935=CIRCLE('',#16190,1.24783954473516);
#5936=CIRCLE('',#16191,0.0555000000000001);
#5937=CIRCLE('',#16192,1.24783954473516);
#5938=CIRCLE('',#16193,0.0555000000000001);
#5939=CIRCLE('',#16194,1.24783954473516);
#5940=CIRCLE('',#16196,1.4);
#5941=CIRCLE('',#16280,0.3);
#5942=CIRCLE('',#16282,0.35);
#5943=CIRCLE('',#16284,0.35);
#5944=CIRCLE('',#16286,0.32);
#5945=CIRCLE('',#16288,0.22);
#5946=CIRCLE('',#16290,0.1954);
#5947=CIRCLE('',#16292,0.1954);
#5948=CIRCLE('',#16294,0.16);
#5949=CIRCLE('',#16392,0.22);
#5950=CIRCLE('',#16394,0.24505);
#5951=CIRCLE('',#16396,0.24505);
#5952=CIRCLE('',#16398,0.175);
#5953=VERTEX_POINT('',#20974);
#5954=VERTEX_POINT('',#20976);
#5955=VERTEX_POINT('',#20981);
#5956=VERTEX_POINT('',#20983);
#5957=VERTEX_POINT('',#20988);
#5958=VERTEX_POINT('',#20990);
#5959=VERTEX_POINT('',#20995);
#5960=VERTEX_POINT('',#20997);
#5961=VERTEX_POINT('',#21002);
#5962=VERTEX_POINT('',#21004);
#5963=VERTEX_POINT('',#21009);
#5964=VERTEX_POINT('',#21011);
#5965=VERTEX_POINT('',#21016);
#5966=VERTEX_POINT('',#21018);
#5967=VERTEX_POINT('',#21023);
#5968=VERTEX_POINT('',#21025);
#5969=VERTEX_POINT('',#21030);
#5970=VERTEX_POINT('',#21032);
#5971=VERTEX_POINT('',#21037);
#5972=VERTEX_POINT('',#21039);
#5973=VERTEX_POINT('',#21044);
#5974=VERTEX_POINT('',#21045);
#5975=VERTEX_POINT('',#21047);
#5976=VERTEX_POINT('',#21049);
#5977=VERTEX_POINT('',#21053);
#5978=VERTEX_POINT('',#21054);
#5979=VERTEX_POINT('',#21056);
#5980=VERTEX_POINT('',#21058);
#5981=VERTEX_POINT('',#21062);
#5982=VERTEX_POINT('',#21063);
#5983=VERTEX_POINT('',#21065);
#5984=VERTEX_POINT('',#21067);
#5985=VERTEX_POINT('',#21070);
#5986=VERTEX_POINT('',#21071);
#5987=VERTEX_POINT('',#21073);
#5988=VERTEX_POINT('',#21075);
#5989=VERTEX_POINT('',#21078);
#5990=VERTEX_POINT('',#21079);
#5991=VERTEX_POINT('',#21081);
#5992=VERTEX_POINT('',#21083);
#5993=VERTEX_POINT('',#21086);
#5994=VERTEX_POINT('',#21087);
#5995=VERTEX_POINT('',#21089);
#5996=VERTEX_POINT('',#21091);
#5997=VERTEX_POINT('',#21101);
#5998=VERTEX_POINT('',#21103);
#5999=VERTEX_POINT('',#21107);
#6000=VERTEX_POINT('',#21109);
#6001=VERTEX_POINT('',#21117);
#6002=VERTEX_POINT('',#21118);
#6003=VERTEX_POINT('',#21120);
#6004=VERTEX_POINT('',#21123);
#6005=VERTEX_POINT('',#21125);
#6006=VERTEX_POINT('',#21127);
#6007=VERTEX_POINT('',#21131);
#6008=VERTEX_POINT('',#21133);
#6009=VERTEX_POINT('',#21141);
#6010=VERTEX_POINT('',#21142);
#6011=VERTEX_POINT('',#21144);
#6012=VERTEX_POINT('',#21147);
#6013=VERTEX_POINT('',#21149);
#6014=VERTEX_POINT('',#21151);
#6015=VERTEX_POINT('',#21155);
#6016=VERTEX_POINT('',#21157);
#6017=VERTEX_POINT('',#21169);
#6018=VERTEX_POINT('',#21171);
#6019=VERTEX_POINT('',#21176);
#6020=VERTEX_POINT('',#21178);
#6021=VERTEX_POINT('',#21187);
#6022=VERTEX_POINT('',#21189);
#6023=VERTEX_POINT('',#21193);
#6024=VERTEX_POINT('',#21197);
#6025=VERTEX_POINT('',#21205);
#6026=VERTEX_POINT('',#21206);
#6027=VERTEX_POINT('',#21208);
#6028=VERTEX_POINT('',#21210);
#6029=VERTEX_POINT('',#21214);
#6030=VERTEX_POINT('',#21216);
#6031=VERTEX_POINT('',#21220);
#6032=VERTEX_POINT('',#21222);
#6033=VERTEX_POINT('',#21232);
#6034=VERTEX_POINT('',#21233);
#6035=VERTEX_POINT('',#21235);
#6036=VERTEX_POINT('',#21237);
#6037=VERTEX_POINT('',#21241);
#6038=VERTEX_POINT('',#21243);
#6039=VERTEX_POINT('',#21247);
#6040=VERTEX_POINT('',#21249);
#6041=VERTEX_POINT('',#21259);
#6042=VERTEX_POINT('',#21261);
#6043=VERTEX_POINT('',#21265);
#6044=VERTEX_POINT('',#21267);
#6045=VERTEX_POINT('',#21271);
#6046=VERTEX_POINT('',#21273);
#6047=VERTEX_POINT('',#21277);
#6048=VERTEX_POINT('',#21279);
#6049=VERTEX_POINT('',#21283);
#6050=VERTEX_POINT('',#21285);
#6051=VERTEX_POINT('',#21289);
#6052=VERTEX_POINT('',#21291);
#6053=VERTEX_POINT('',#21295);
#6054=VERTEX_POINT('',#21297);
#6055=VERTEX_POINT('',#21301);
#6056=VERTEX_POINT('',#21303);
#6057=VERTEX_POINT('',#21307);
#6058=VERTEX_POINT('',#21309);
#6059=VERTEX_POINT('',#21313);
#6060=VERTEX_POINT('',#21314);
#6061=VERTEX_POINT('',#21316);
#6062=VERTEX_POINT('',#21318);
#6063=VERTEX_POINT('',#21322);
#6064=VERTEX_POINT('',#21323);
#6065=VERTEX_POINT('',#21325);
#6066=VERTEX_POINT('',#21327);
#6067=VERTEX_POINT('',#21331);
#6068=VERTEX_POINT('',#21333);
#6069=VERTEX_POINT('',#21337);
#6070=VERTEX_POINT('',#21339);
#6071=VERTEX_POINT('',#21343);
#6072=VERTEX_POINT('',#21345);
#6073=VERTEX_POINT('',#21350);
#6074=VERTEX_POINT('',#21354);
#6075=VERTEX_POINT('',#21364);
#6076=VERTEX_POINT('',#21366);
#6077=VERTEX_POINT('',#21370);
#6078=VERTEX_POINT('',#21372);
#6079=VERTEX_POINT('',#21379);
#6080=VERTEX_POINT('',#21380);
#6081=VERTEX_POINT('',#21382);
#6082=VERTEX_POINT('',#21384);
#6083=VERTEX_POINT('',#21388);
#6084=VERTEX_POINT('',#21389);
#6085=VERTEX_POINT('',#21391);
#6086=VERTEX_POINT('',#21393);
#6087=VERTEX_POINT('',#21397);
#6088=VERTEX_POINT('',#21398);
#6089=VERTEX_POINT('',#21400);
#6090=VERTEX_POINT('',#21402);
#6091=VERTEX_POINT('',#21406);
#6092=VERTEX_POINT('',#21407);
#6093=VERTEX_POINT('',#21409);
#6094=VERTEX_POINT('',#21411);
#6095=VERTEX_POINT('',#21419);
#6096=VERTEX_POINT('',#21430);
#6097=VERTEX_POINT('',#21432);
#6098=VERTEX_POINT('',#21436);
#6099=VERTEX_POINT('',#21443);
#6100=VERTEX_POINT('',#21444);
#6101=VERTEX_POINT('',#21446);
#6102=VERTEX_POINT('',#21448);
#6103=VERTEX_POINT('',#21452);
#6104=VERTEX_POINT('',#21453);
#6105=VERTEX_POINT('',#21455);
#6106=VERTEX_POINT('',#21457);
#6107=VERTEX_POINT('',#21461);
#6108=VERTEX_POINT('',#21462);
#6109=VERTEX_POINT('',#21464);
#6110=VERTEX_POINT('',#21466);
#6111=VERTEX_POINT('',#21470);
#6112=VERTEX_POINT('',#21471);
#6113=VERTEX_POINT('',#21473);
#6114=VERTEX_POINT('',#21475);
#6115=VERTEX_POINT('',#21483);
#6116=VERTEX_POINT('',#21494);
#6117=VERTEX_POINT('',#21498);
#6118=VERTEX_POINT('',#21501);
#6119=VERTEX_POINT('',#21507);
#6120=VERTEX_POINT('',#21508);
#6121=VERTEX_POINT('',#21510);
#6122=VERTEX_POINT('',#21512);
#6123=VERTEX_POINT('',#21516);
#6124=VERTEX_POINT('',#21517);
#6125=VERTEX_POINT('',#21519);
#6126=VERTEX_POINT('',#21521);
#6127=VERTEX_POINT('',#21525);
#6128=VERTEX_POINT('',#21527);
#6129=VERTEX_POINT('',#21531);
#6130=VERTEX_POINT('',#21533);
#6131=VERTEX_POINT('',#21535);
#6132=VERTEX_POINT('',#21537);
#6133=VERTEX_POINT('',#21539);
#6134=VERTEX_POINT('',#21542);
#6135=VERTEX_POINT('',#21544);
#6136=VERTEX_POINT('',#21548);
#6137=VERTEX_POINT('',#21550);
#6138=VERTEX_POINT('',#21552);
#6139=VERTEX_POINT('',#21554);
#6140=VERTEX_POINT('',#21558);
#6141=VERTEX_POINT('',#21560);
#6142=VERTEX_POINT('',#21568);
#6143=VERTEX_POINT('',#21572);
#6144=VERTEX_POINT('',#21576);
#6145=VERTEX_POINT('',#21580);
#6146=VERTEX_POINT('',#21584);
#6147=VERTEX_POINT('',#21588);
#6148=VERTEX_POINT('',#21590);
#6149=VERTEX_POINT('',#21594);
#6150=VERTEX_POINT('',#21596);
#6151=VERTEX_POINT('',#21600);
#6152=VERTEX_POINT('',#21602);
#6153=VERTEX_POINT('',#21606);
#6154=VERTEX_POINT('',#21608);
#6155=VERTEX_POINT('',#21612);
#6156=VERTEX_POINT('',#21614);
#6157=VERTEX_POINT('',#21618);
#6158=VERTEX_POINT('',#21619);
#6159=VERTEX_POINT('',#21621);
#6160=VERTEX_POINT('',#21623);
#6161=VERTEX_POINT('',#21627);
#6162=VERTEX_POINT('',#21629);
#6163=VERTEX_POINT('',#21633);
#6164=VERTEX_POINT('',#21635);
#6165=VERTEX_POINT('',#21648);
#6166=VERTEX_POINT('',#21650);
#6167=VERTEX_POINT('',#21654);
#6168=VERTEX_POINT('',#21656);
#6169=VERTEX_POINT('',#21663);
#6170=VERTEX_POINT('',#21665);
#6171=VERTEX_POINT('',#21669);
#6172=VERTEX_POINT('',#21671);
#6173=VERTEX_POINT('',#21678);
#6174=VERTEX_POINT('',#21680);
#6175=VERTEX_POINT('',#21684);
#6176=VERTEX_POINT('',#21686);
#6177=VERTEX_POINT('',#21693);
#6178=VERTEX_POINT('',#21695);
#6179=VERTEX_POINT('',#21699);
#6180=VERTEX_POINT('',#21701);
#6181=VERTEX_POINT('',#21708);
#6182=VERTEX_POINT('',#21710);
#6183=VERTEX_POINT('',#21714);
#6184=VERTEX_POINT('',#21716);
#6185=VERTEX_POINT('',#21723);
#6186=VERTEX_POINT('',#21724);
#6187=VERTEX_POINT('',#21726);
#6188=VERTEX_POINT('',#21728);
#6189=VERTEX_POINT('',#21732);
#6190=VERTEX_POINT('',#21733);
#6191=VERTEX_POINT('',#21735);
#6192=VERTEX_POINT('',#21737);
#6193=VERTEX_POINT('',#21741);
#6194=VERTEX_POINT('',#21742);
#6195=VERTEX_POINT('',#21744);
#6196=VERTEX_POINT('',#21746);
#6197=VERTEX_POINT('',#21750);
#6198=VERTEX_POINT('',#21751);
#6199=VERTEX_POINT('',#21753);
#6200=VERTEX_POINT('',#21755);
#6201=VERTEX_POINT('',#21763);
#6202=VERTEX_POINT('',#21774);
#6203=VERTEX_POINT('',#21776);
#6204=VERTEX_POINT('',#21780);
#6205=VERTEX_POINT('',#21787);
#6206=VERTEX_POINT('',#21788);
#6207=VERTEX_POINT('',#21790);
#6208=VERTEX_POINT('',#21792);
#6209=VERTEX_POINT('',#21796);
#6210=VERTEX_POINT('',#21798);
#6211=VERTEX_POINT('',#21802);
#6212=VERTEX_POINT('',#21803);
#6213=VERTEX_POINT('',#21805);
#6214=VERTEX_POINT('',#21807);
#6215=VERTEX_POINT('',#21811);
#6216=VERTEX_POINT('',#21813);
#6217=VERTEX_POINT('',#21817);
#6218=VERTEX_POINT('',#21818);
#6219=VERTEX_POINT('',#21820);
#6220=VERTEX_POINT('',#21822);
#6221=VERTEX_POINT('',#21826);
#6222=VERTEX_POINT('',#21828);
#6223=VERTEX_POINT('',#21832);
#6224=VERTEX_POINT('',#21833);
#6225=VERTEX_POINT('',#21835);
#6226=VERTEX_POINT('',#21837);
#6227=VERTEX_POINT('',#21841);
#6228=VERTEX_POINT('',#21843);
#6229=VERTEX_POINT('',#21847);
#6230=VERTEX_POINT('',#21849);
#6231=VERTEX_POINT('',#21853);
#6232=VERTEX_POINT('',#21855);
#6233=VERTEX_POINT('',#21859);
#6234=VERTEX_POINT('',#21861);
#6235=VERTEX_POINT('',#21866);
#6236=VERTEX_POINT('',#21873);
#6237=VERTEX_POINT('',#21876);
#6238=VERTEX_POINT('',#21881);
#6239=VERTEX_POINT('',#21892);
#6240=VERTEX_POINT('',#21893);
#6241=VERTEX_POINT('',#21895);
#6242=VERTEX_POINT('',#21897);
#6243=VERTEX_POINT('',#21901);
#6244=VERTEX_POINT('',#21902);
#6245=VERTEX_POINT('',#21904);
#6246=VERTEX_POINT('',#21906);
#6247=VERTEX_POINT('',#21910);
#6248=VERTEX_POINT('',#21911);
#6249=VERTEX_POINT('',#21913);
#6250=VERTEX_POINT('',#21915);
#6251=VERTEX_POINT('',#21925);
#6252=VERTEX_POINT('',#21927);
#6253=VERTEX_POINT('',#21931);
#6254=VERTEX_POINT('',#21935);
#6255=VERTEX_POINT('',#21943);
#6256=VERTEX_POINT('',#21945);
#6257=VERTEX_POINT('',#21949);
#6258=VERTEX_POINT('',#21952);
#6259=VERTEX_POINT('',#21956);
#6260=VERTEX_POINT('',#21958);
#6261=VERTEX_POINT('',#21962);
#6262=VERTEX_POINT('',#21965);
#6263=VERTEX_POINT('',#21969);
#6264=VERTEX_POINT('',#21971);
#6265=VERTEX_POINT('',#21975);
#6266=VERTEX_POINT('',#21978);
#6267=VERTEX_POINT('',#21982);
#6268=VERTEX_POINT('',#21984);
#6269=VERTEX_POINT('',#21988);
#6270=VERTEX_POINT('',#21991);
#6271=VERTEX_POINT('',#21995);
#6272=VERTEX_POINT('',#21997);
#6273=VERTEX_POINT('',#22002);
#6274=VERTEX_POINT('',#22004);
#6275=VERTEX_POINT('',#22009);
#6276=VERTEX_POINT('',#22010);
#6277=VERTEX_POINT('',#22012);
#6278=VERTEX_POINT('',#22014);
#6279=VERTEX_POINT('',#22018);
#6280=VERTEX_POINT('',#22020);
#6281=VERTEX_POINT('',#22024);
#6282=VERTEX_POINT('',#22026);
#6283=VERTEX_POINT('',#22036);
#6284=VERTEX_POINT('',#22038);
#6285=VERTEX_POINT('',#22042);
#6286=VERTEX_POINT('',#22044);
#6287=VERTEX_POINT('',#22051);
#6288=VERTEX_POINT('',#22053);
#6289=VERTEX_POINT('',#22057);
#6290=VERTEX_POINT('',#22059);
#6291=VERTEX_POINT('',#22066);
#6292=VERTEX_POINT('',#22068);
#6293=VERTEX_POINT('',#22072);
#6294=VERTEX_POINT('',#22075);
#6295=VERTEX_POINT('',#22079);
#6296=VERTEX_POINT('',#22081);
#6297=VERTEX_POINT('',#22085);
#6298=VERTEX_POINT('',#22088);
#6299=VERTEX_POINT('',#22092);
#6300=VERTEX_POINT('',#22094);
#6301=VERTEX_POINT('',#22098);
#6302=VERTEX_POINT('',#22101);
#6303=VERTEX_POINT('',#22105);
#6304=VERTEX_POINT('',#22107);
#6305=VERTEX_POINT('',#22111);
#6306=VERTEX_POINT('',#22114);
#6307=VERTEX_POINT('',#22118);
#6308=VERTEX_POINT('',#22120);
#6309=VERTEX_POINT('',#22125);
#6310=VERTEX_POINT('',#22127);
#6311=VERTEX_POINT('',#22132);
#6312=VERTEX_POINT('',#22133);
#6313=VERTEX_POINT('',#22135);
#6314=VERTEX_POINT('',#22137);
#6315=VERTEX_POINT('',#22141);
#6316=VERTEX_POINT('',#22143);
#6317=VERTEX_POINT('',#22147);
#6318=VERTEX_POINT('',#22149);
#6319=VERTEX_POINT('',#22159);
#6320=VERTEX_POINT('',#22161);
#6321=VERTEX_POINT('',#22165);
#6322=VERTEX_POINT('',#22167);
#6323=VERTEX_POINT('',#22174);
#6324=VERTEX_POINT('',#22176);
#6325=VERTEX_POINT('',#22180);
#6326=VERTEX_POINT('',#22182);
#6327=VERTEX_POINT('',#22189);
#6328=VERTEX_POINT('',#22191);
#6329=VERTEX_POINT('',#22195);
#6330=VERTEX_POINT('',#22198);
#6331=VERTEX_POINT('',#22202);
#6332=VERTEX_POINT('',#22204);
#6333=VERTEX_POINT('',#22208);
#6334=VERTEX_POINT('',#22211);
#6335=VERTEX_POINT('',#22215);
#6336=VERTEX_POINT('',#22216);
#6337=VERTEX_POINT('',#22218);
#6338=VERTEX_POINT('',#22220);
#6339=VERTEX_POINT('',#22224);
#6340=VERTEX_POINT('',#22226);
#6341=VERTEX_POINT('',#22230);
#6342=VERTEX_POINT('',#22232);
#6343=VERTEX_POINT('',#22242);
#6344=VERTEX_POINT('',#22243);
#6345=VERTEX_POINT('',#22245);
#6346=VERTEX_POINT('',#22247);
#6347=VERTEX_POINT('',#22251);
#6348=VERTEX_POINT('',#22253);
#6349=VERTEX_POINT('',#22257);
#6350=VERTEX_POINT('',#22259);
#6351=VERTEX_POINT('',#22269);
#6352=VERTEX_POINT('',#22271);
#6353=VERTEX_POINT('',#22275);
#6354=VERTEX_POINT('',#22277);
#6355=VERTEX_POINT('',#22281);
#6356=VERTEX_POINT('',#22282);
#6357=VERTEX_POINT('',#22284);
#6358=VERTEX_POINT('',#22286);
#6359=VERTEX_POINT('',#22290);
#6360=VERTEX_POINT('',#22292);
#6361=VERTEX_POINT('',#22296);
#6362=VERTEX_POINT('',#22298);
#6363=VERTEX_POINT('',#22308);
#6364=VERTEX_POINT('',#22310);
#6365=VERTEX_POINT('',#22314);
#6366=VERTEX_POINT('',#22316);
#6367=VERTEX_POINT('',#22320);
#6368=VERTEX_POINT('',#22321);
#6369=VERTEX_POINT('',#22323);
#6370=VERTEX_POINT('',#22325);
#6371=VERTEX_POINT('',#22329);
#6372=VERTEX_POINT('',#22331);
#6373=VERTEX_POINT('',#22335);
#6374=VERTEX_POINT('',#22337);
#6375=VERTEX_POINT('',#22347);
#6376=VERTEX_POINT('',#22349);
#6377=VERTEX_POINT('',#22353);
#6378=VERTEX_POINT('',#22355);
#6379=VERTEX_POINT('',#22359);
#6380=VERTEX_POINT('',#22361);
#6381=VERTEX_POINT('',#22365);
#6382=VERTEX_POINT('',#22367);
#6383=VERTEX_POINT('',#22371);
#6384=VERTEX_POINT('',#22372);
#6385=VERTEX_POINT('',#22374);
#6386=VERTEX_POINT('',#22376);
#6387=VERTEX_POINT('',#22380);
#6388=VERTEX_POINT('',#22382);
#6389=VERTEX_POINT('',#22386);
#6390=VERTEX_POINT('',#22388);
#6391=VERTEX_POINT('',#22399);
#6392=VERTEX_POINT('',#22400);
#6393=VERTEX_POINT('',#22403);
#6394=VERTEX_POINT('',#22405);
#6395=VERTEX_POINT('',#22409);
#6396=VERTEX_POINT('',#22413);
#6397=VERTEX_POINT('',#22415);
#6398=VERTEX_POINT('',#22419);
#6399=VERTEX_POINT('',#22424);
#6400=VERTEX_POINT('',#22428);
#6401=VERTEX_POINT('',#22434);
#6402=VERTEX_POINT('',#22435);
#6403=VERTEX_POINT('',#22438);
#6404=VERTEX_POINT('',#22440);
#6405=VERTEX_POINT('',#22444);
#6406=VERTEX_POINT('',#22448);
#6407=VERTEX_POINT('',#22450);
#6408=VERTEX_POINT('',#22453);
#6409=VERTEX_POINT('',#22457);
#6410=VERTEX_POINT('',#22461);
#6411=VERTEX_POINT('',#22469);
#6412=VERTEX_POINT('',#22470);
#6413=VERTEX_POINT('',#22473);
#6414=VERTEX_POINT('',#22474);
#6415=VERTEX_POINT('',#22477);
#6416=VERTEX_POINT('',#22478);
#6417=VERTEX_POINT('',#22481);
#6418=VERTEX_POINT('',#22482);
#6419=VERTEX_POINT('',#22485);
#6420=VERTEX_POINT('',#22486);
#6421=VERTEX_POINT('',#22489);
#6422=VERTEX_POINT('',#22490);
#6423=VERTEX_POINT('',#22493);
#6424=VERTEX_POINT('',#22494);
#6425=VERTEX_POINT('',#22497);
#6426=VERTEX_POINT('',#22498);
#6427=VERTEX_POINT('',#22502);
#6428=VERTEX_POINT('',#22503);
#6429=VERTEX_POINT('',#22526);
#6430=VERTEX_POINT('',#22528);
#6431=VERTEX_POINT('',#22553);
#6432=VERTEX_POINT('',#22555);
#6433=VERTEX_POINT('',#22578);
#6434=VERTEX_POINT('',#22580);
#6435=VERTEX_POINT('',#22603);
#6436=VERTEX_POINT('',#22605);
#6437=VERTEX_POINT('',#22618);
#6438=VERTEX_POINT('',#22621);
#6439=VERTEX_POINT('',#22634);
#6440=VERTEX_POINT('',#22636);
#6441=VERTEX_POINT('',#22659);
#6442=VERTEX_POINT('',#22661);
#6443=VERTEX_POINT('',#22684);
#6444=VERTEX_POINT('',#22686);
#6445=VERTEX_POINT('',#22709);
#6446=VERTEX_POINT('',#22711);
#6447=VERTEX_POINT('',#22736);
#6448=VERTEX_POINT('',#22740);
#6449=VERTEX_POINT('',#22765);
#6450=VERTEX_POINT('',#22769);
#6451=VERTEX_POINT('',#22794);
#6452=VERTEX_POINT('',#22798);
#6453=VERTEX_POINT('',#22799);
#6454=VERTEX_POINT('',#22826);
#6455=VERTEX_POINT('',#22830);
#6456=VERTEX_POINT('',#22855);
#6457=VERTEX_POINT('',#22859);
#6458=VERTEX_POINT('',#22884);
#6459=VERTEX_POINT('',#22888);
#6460=VERTEX_POINT('',#22913);
#6461=VERTEX_POINT('',#22916);
#6462=VERTEX_POINT('',#22918);
#6463=VERTEX_POINT('',#22950);
#6464=VERTEX_POINT('',#22952);
#6465=VERTEX_POINT('',#22955);
#6466=VERTEX_POINT('',#22959);
#6467=VERTEX_POINT('',#22964);
#6468=VERTEX_POINT('',#22966);
#6469=VERTEX_POINT('',#22969);
#6470=VERTEX_POINT('',#22973);
#6471=VERTEX_POINT('',#22984);
#6472=VERTEX_POINT('',#22985);
#6473=VERTEX_POINT('',#22987);
#6474=VERTEX_POINT('',#22989);
#6475=VERTEX_POINT('',#22993);
#6476=VERTEX_POINT('',#22995);
#6477=VERTEX_POINT('',#22999);
#6478=VERTEX_POINT('',#23001);
#6479=VERTEX_POINT('',#23005);
#6480=VERTEX_POINT('',#23007);
#6481=VERTEX_POINT('',#23011);
#6482=VERTEX_POINT('',#23013);
#6483=VERTEX_POINT('',#23022);
#6484=VERTEX_POINT('',#23024);
#6485=VERTEX_POINT('',#23027);
#6486=VERTEX_POINT('',#23032);
#6487=VERTEX_POINT('',#23035);
#6488=VERTEX_POINT('',#23039);
#6489=VERTEX_POINT('',#23043);
#6490=VERTEX_POINT('',#23047);
#6491=VERTEX_POINT('',#23050);
#6492=VERTEX_POINT('',#23054);
#6493=VERTEX_POINT('',#23062);
#6494=VERTEX_POINT('',#23063);
#6495=VERTEX_POINT('',#23066);
#6496=VERTEX_POINT('',#23068);
#6497=VERTEX_POINT('',#23072);
#6498=VERTEX_POINT('',#23076);
#6499=VERTEX_POINT('',#23078);
#6500=VERTEX_POINT('',#23082);
#6501=VERTEX_POINT('',#23087);
#6502=VERTEX_POINT('',#23091);
#6503=VERTEX_POINT('',#23097);
#6504=VERTEX_POINT('',#23098);
#6505=VERTEX_POINT('',#23101);
#6506=VERTEX_POINT('',#23103);
#6507=VERTEX_POINT('',#23107);
#6508=VERTEX_POINT('',#23111);
#6509=VERTEX_POINT('',#23113);
#6510=VERTEX_POINT('',#23116);
#6511=VERTEX_POINT('',#23120);
#6512=VERTEX_POINT('',#23124);
#6513=VERTEX_POINT('',#23132);
#6514=VERTEX_POINT('',#23133);
#6515=VERTEX_POINT('',#23136);
#6516=VERTEX_POINT('',#23137);
#6517=VERTEX_POINT('',#23140);
#6518=VERTEX_POINT('',#23141);
#6519=VERTEX_POINT('',#23144);
#6520=VERTEX_POINT('',#23145);
#6521=VERTEX_POINT('',#23148);
#6522=VERTEX_POINT('',#23149);
#6523=VERTEX_POINT('',#23152);
#6524=VERTEX_POINT('',#23153);
#6525=VERTEX_POINT('',#23156);
#6526=VERTEX_POINT('',#23157);
#6527=VERTEX_POINT('',#23161);
#6528=VERTEX_POINT('',#23162);
#6529=VERTEX_POINT('',#23185);
#6530=VERTEX_POINT('',#23187);
#6531=VERTEX_POINT('',#23212);
#6532=VERTEX_POINT('',#23214);
#6533=VERTEX_POINT('',#23237);
#6534=VERTEX_POINT('',#23239);
#6535=VERTEX_POINT('',#23262);
#6536=VERTEX_POINT('',#23264);
#6537=VERTEX_POINT('',#23267);
#6538=VERTEX_POINT('',#23269);
#6539=VERTEX_POINT('',#23292);
#6540=VERTEX_POINT('',#23294);
#6541=VERTEX_POINT('',#23317);
#6542=VERTEX_POINT('',#23319);
#6543=VERTEX_POINT('',#23342);
#6544=VERTEX_POINT('',#23344);
#6545=VERTEX_POINT('',#23369);
#6546=VERTEX_POINT('',#23373);
#6547=VERTEX_POINT('',#23398);
#6548=VERTEX_POINT('',#23402);
#6549=VERTEX_POINT('',#23427);
#6550=VERTEX_POINT('',#23429);
#6551=VERTEX_POINT('',#23433);
#6552=VERTEX_POINT('',#23458);
#6553=VERTEX_POINT('',#23462);
#6554=VERTEX_POINT('',#23487);
#6555=VERTEX_POINT('',#23491);
#6556=VERTEX_POINT('',#23516);
#6557=VERTEX_POINT('',#23519);
#6558=VERTEX_POINT('',#23521);
#6559=VERTEX_POINT('',#23553);
#6560=VERTEX_POINT('',#23555);
#6561=VERTEX_POINT('',#23558);
#6562=VERTEX_POINT('',#23562);
#6563=VERTEX_POINT('',#23567);
#6564=VERTEX_POINT('',#23569);
#6565=VERTEX_POINT('',#23572);
#6566=VERTEX_POINT('',#23576);
#6567=VERTEX_POINT('',#23587);
#6568=VERTEX_POINT('',#23590);
#6569=VERTEX_POINT('',#23594);
#6570=VERTEX_POINT('',#23598);
#6571=VERTEX_POINT('',#23602);
#6572=VERTEX_POINT('',#23605);
#6573=VERTEX_POINT('',#23609);
#6574=VERTEX_POINT('',#23613);
#6575=VERTEX_POINT('',#23618);
#6576=VERTEX_POINT('',#23619);
#6577=VERTEX_POINT('',#23621);
#6578=VERTEX_POINT('',#23623);
#6579=VERTEX_POINT('',#23627);
#6580=VERTEX_POINT('',#23629);
#6581=VERTEX_POINT('',#23633);
#6582=VERTEX_POINT('',#23635);
#6583=VERTEX_POINT('',#23639);
#6584=VERTEX_POINT('',#23641);
#6585=VERTEX_POINT('',#23645);
#6586=VERTEX_POINT('',#23647);
#6587=VERTEX_POINT('',#23658);
#6588=VERTEX_POINT('',#23660);
#6589=VERTEX_POINT('',#23664);
#6590=VERTEX_POINT('',#23666);
#6591=VERTEX_POINT('',#23670);
#6592=VERTEX_POINT('',#23671);
#6593=VERTEX_POINT('',#23674);
#6594=VERTEX_POINT('',#23675);
#6595=VERTEX_POINT('',#23677);
#6596=VERTEX_POINT('',#23681);
#6597=VERTEX_POINT('',#23682);
#6598=VERTEX_POINT('',#23684);
#6599=VERTEX_POINT('',#23688);
#6600=VERTEX_POINT('',#23689);
#6601=VERTEX_POINT('',#23691);
#6602=VERTEX_POINT('',#23698);
#6603=VERTEX_POINT('',#23699);
#6604=VERTEX_POINT('',#23701);
#6605=VERTEX_POINT('',#23708);
#6606=VERTEX_POINT('',#23709);
#6607=VERTEX_POINT('',#23711);
#6608=VERTEX_POINT('',#23713);
#6609=VERTEX_POINT('',#23716);
#6610=VERTEX_POINT('',#23718);
#6611=VERTEX_POINT('',#23720);
#6612=VERTEX_POINT('',#23722);
#6613=VERTEX_POINT('',#23725);
#6614=VERTEX_POINT('',#23727);
#6615=VERTEX_POINT('',#23736);
#6616=VERTEX_POINT('',#23737);
#6617=VERTEX_POINT('',#23739);
#6618=VERTEX_POINT('',#23741);
#6619=VERTEX_POINT('',#23745);
#6620=VERTEX_POINT('',#23747);
#6621=VERTEX_POINT('',#23751);
#6622=VERTEX_POINT('',#23753);
#6623=VERTEX_POINT('',#23761);
#6624=VERTEX_POINT('',#23765);
#6625=VERTEX_POINT('',#23769);
#6626=VERTEX_POINT('',#23770);
#6627=VERTEX_POINT('',#23775);
#6628=VERTEX_POINT('',#23779);
#6629=VERTEX_POINT('',#23787);
#6630=VERTEX_POINT('',#23789);
#6631=VERTEX_POINT('',#23793);
#6632=VERTEX_POINT('',#23796);
#6633=VERTEX_POINT('',#23797);
#6634=VERTEX_POINT('',#23799);
#6635=VERTEX_POINT('',#23803);
#6636=VERTEX_POINT('',#23804);
#6637=VERTEX_POINT('',#23815);
#6638=VERTEX_POINT('',#23844);
#6639=VERTEX_POINT('',#23881);
#6640=VERTEX_POINT('',#23916);
#6641=VERTEX_POINT('',#23918);
#6642=VERTEX_POINT('',#23929);
#6643=VERTEX_POINT('',#23959);
#6644=VERTEX_POINT('',#23961);
#6645=VERTEX_POINT('',#23964);
#6646=VERTEX_POINT('',#23965);
#6647=VERTEX_POINT('',#23984);
#6648=VERTEX_POINT('',#24005);
#6649=VERTEX_POINT('',#24006);
#6650=VERTEX_POINT('',#24025);
#6651=VERTEX_POINT('',#24046);
#6652=VERTEX_POINT('',#24047);
#6653=VERTEX_POINT('',#24066);
#6654=VERTEX_POINT('',#24087);
#6655=VERTEX_POINT('',#24088);
#6656=VERTEX_POINT('',#24107);
#6657=VERTEX_POINT('',#24129);
#6658=VERTEX_POINT('',#24166);
#6659=VERTEX_POINT('',#24203);
#6660=VERTEX_POINT('',#24240);
#6661=VERTEX_POINT('',#24277);
#6662=VERTEX_POINT('',#24280);
#6663=VERTEX_POINT('',#24283);
#6664=VERTEX_POINT('',#24287);
#6665=VERTEX_POINT('',#24295);
#6666=VERTEX_POINT('',#24297);
#6667=VERTEX_POINT('',#24301);
#6668=VERTEX_POINT('',#24303);
#6669=VERTEX_POINT('',#24310);
#6670=VERTEX_POINT('',#24311);
#6671=VERTEX_POINT('',#24313);
#6672=VERTEX_POINT('',#24315);
#6673=VERTEX_POINT('',#24319);
#6674=VERTEX_POINT('',#24321);
#6675=VERTEX_POINT('',#24325);
#6676=VERTEX_POINT('',#24327);
#6677=VERTEX_POINT('',#24331);
#6678=VERTEX_POINT('',#24333);
#6679=VERTEX_POINT('',#24337);
#6680=VERTEX_POINT('',#24339);
#6681=VERTEX_POINT('',#24348);
#6682=VERTEX_POINT('',#24351);
#6683=VERTEX_POINT('',#24354);
#6684=VERTEX_POINT('',#24358);
#6685=VERTEX_POINT('',#24362);
#6686=VERTEX_POINT('',#24366);
#6687=VERTEX_POINT('',#24369);
#6688=VERTEX_POINT('',#24376);
#6689=VERTEX_POINT('',#24377);
#6690=VERTEX_POINT('',#24379);
#6691=VERTEX_POINT('',#24381);
#6692=VERTEX_POINT('',#24385);
#6693=VERTEX_POINT('',#24387);
#6694=VERTEX_POINT('',#24391);
#6695=VERTEX_POINT('',#24393);
#6696=VERTEX_POINT('',#24397);
#6697=VERTEX_POINT('',#24399);
#6698=VERTEX_POINT('',#24403);
#6699=VERTEX_POINT('',#24405);
#6700=VERTEX_POINT('',#24414);
#6701=VERTEX_POINT('',#24417);
#6702=VERTEX_POINT('',#24420);
#6703=VERTEX_POINT('',#24424);
#6704=VERTEX_POINT('',#24428);
#6705=VERTEX_POINT('',#24432);
#6706=VERTEX_POINT('',#24435);
#6707=VERTEX_POINT('',#24443);
#6708=VERTEX_POINT('',#24445);
#6709=VERTEX_POINT('',#24450);
#6710=VERTEX_POINT('',#24452);
#6711=VERTEX_POINT('',#24455);
#6712=VERTEX_POINT('',#24457);
#6713=VERTEX_POINT('',#24462);
#6714=VERTEX_POINT('',#24466);
#6715=VERTEX_POINT('',#24468);
#6716=VERTEX_POINT('',#24473);
#6717=VERTEX_POINT('',#24480);
#6718=VERTEX_POINT('',#24482);
#6719=VERTEX_POINT('',#24486);
#6720=VERTEX_POINT('',#24489);
#6721=VERTEX_POINT('',#24493);
#6722=VERTEX_POINT('',#24495);
#6723=VERTEX_POINT('',#24502);
#6724=VERTEX_POINT('',#24504);
#6725=VERTEX_POINT('',#24508);
#6726=VERTEX_POINT('',#24510);
#6727=VERTEX_POINT('',#24517);
#6728=VERTEX_POINT('',#24519);
#6729=VERTEX_POINT('',#24526);
#6730=VERTEX_POINT('',#24528);
#6731=VERTEX_POINT('',#24535);
#6732=VERTEX_POINT('',#24537);
#6733=VERTEX_POINT('',#24541);
#6734=VERTEX_POINT('',#24543);
#6735=VERTEX_POINT('',#24550);
#6736=VERTEX_POINT('',#24552);
#6737=VERTEX_POINT('',#24559);
#6738=VERTEX_POINT('',#24560);
#6739=VERTEX_POINT('',#24564);
#6740=VERTEX_POINT('',#24575);
#6741=VERTEX_POINT('',#24577);
#6742=VERTEX_POINT('',#24579);
#6743=VERTEX_POINT('',#24616);
#6744=VERTEX_POINT('',#24631);
#6745=VERTEX_POINT('',#24632);
#6746=VERTEX_POINT('',#24636);
#6747=VERTEX_POINT('',#24647);
#6748=VERTEX_POINT('',#24649);
#6749=VERTEX_POINT('',#24651);
#6750=VERTEX_POINT('',#24688);
#6751=VERTEX_POINT('',#24703);
#6752=VERTEX_POINT('',#24705);
#6753=VERTEX_POINT('',#24709);
#6754=VERTEX_POINT('',#24711);
#6755=VERTEX_POINT('',#24718);
#6756=VERTEX_POINT('',#24719);
#6757=VERTEX_POINT('',#24730);
#6758=VERTEX_POINT('',#24759);
#6759=VERTEX_POINT('',#24761);
#6760=VERTEX_POINT('',#24772);
#6761=VERTEX_POINT('',#24783);
#6762=VERTEX_POINT('',#24805);
#6763=VERTEX_POINT('',#24806);
#6764=VERTEX_POINT('',#24843);
#6765=VERTEX_POINT('',#24845);
#6766=VERTEX_POINT('',#24856);
#6767=VERTEX_POINT('',#24886);
#6768=VERTEX_POINT('',#24889);
#6769=VERTEX_POINT('',#24892);
#6770=VERTEX_POINT('',#24893);
#6771=VERTEX_POINT('',#24912);
#6772=VERTEX_POINT('',#24933);
#6773=VERTEX_POINT('',#24934);
#6774=VERTEX_POINT('',#24953);
#6775=VERTEX_POINT('',#24975);
#6776=VERTEX_POINT('',#24977);
#6777=VERTEX_POINT('',#25015);
#6778=VERTEX_POINT('',#25016);
#6779=VERTEX_POINT('',#25055);
#6780=VERTEX_POINT('',#25058);
#6781=VERTEX_POINT('',#25063);
#6782=VERTEX_POINT('',#25065);
#6783=VERTEX_POINT('',#25066);
#6784=VERTEX_POINT('',#25068);
#6785=VERTEX_POINT('',#25070);
#6786=VERTEX_POINT('',#25072);
#6787=VERTEX_POINT('',#25074);
#6788=VERTEX_POINT('',#25076);
#6789=VERTEX_POINT('',#25078);
#6790=VERTEX_POINT('',#25080);
#6791=VERTEX_POINT('',#25082);
#6792=VERTEX_POINT('',#25084);
#6793=VERTEX_POINT('',#25086);
#6794=VERTEX_POINT('',#25088);
#6795=VERTEX_POINT('',#25090);
#6796=VERTEX_POINT('',#25092);
#6797=VERTEX_POINT('',#25094);
#6798=VERTEX_POINT('',#25096);
#6799=VERTEX_POINT('',#25098);
#6800=VERTEX_POINT('',#25100);
#6801=VERTEX_POINT('',#25102);
#6802=VERTEX_POINT('',#25104);
#6803=VERTEX_POINT('',#25106);
#6804=VERTEX_POINT('',#25108);
#6805=VERTEX_POINT('',#25110);
#6806=VERTEX_POINT('',#25112);
#6807=VERTEX_POINT('',#25114);
#6808=VERTEX_POINT('',#25116);
#6809=VERTEX_POINT('',#25118);
#6810=VERTEX_POINT('',#25120);
#6811=VERTEX_POINT('',#25122);
#6812=VERTEX_POINT('',#25124);
#6813=VERTEX_POINT('',#25126);
#6814=VERTEX_POINT('',#25128);
#6815=VERTEX_POINT('',#25130);
#6816=VERTEX_POINT('',#25132);
#6817=VERTEX_POINT('',#25134);
#6818=VERTEX_POINT('',#25136);
#6819=VERTEX_POINT('',#25138);
#6820=VERTEX_POINT('',#25140);
#6821=VERTEX_POINT('',#25142);
#6822=VERTEX_POINT('',#25146);
#6823=VERTEX_POINT('',#25151);
#6824=VERTEX_POINT('',#25153);
#6825=VERTEX_POINT('',#25154);
#6826=VERTEX_POINT('',#25156);
#6827=VERTEX_POINT('',#25158);
#6828=VERTEX_POINT('',#25160);
#6829=VERTEX_POINT('',#25162);
#6830=VERTEX_POINT('',#25164);
#6831=VERTEX_POINT('',#25166);
#6832=VERTEX_POINT('',#25168);
#6833=VERTEX_POINT('',#25170);
#6834=VERTEX_POINT('',#25172);
#6835=VERTEX_POINT('',#25174);
#6836=VERTEX_POINT('',#25176);
#6837=VERTEX_POINT('',#25178);
#6838=VERTEX_POINT('',#25180);
#6839=VERTEX_POINT('',#25182);
#6840=VERTEX_POINT('',#25184);
#6841=VERTEX_POINT('',#25186);
#6842=VERTEX_POINT('',#25188);
#6843=VERTEX_POINT('',#25190);
#6844=VERTEX_POINT('',#25192);
#6845=VERTEX_POINT('',#25194);
#6846=VERTEX_POINT('',#25196);
#6847=VERTEX_POINT('',#25198);
#6848=VERTEX_POINT('',#25200);
#6849=VERTEX_POINT('',#25202);
#6850=VERTEX_POINT('',#25204);
#6851=VERTEX_POINT('',#25206);
#6852=VERTEX_POINT('',#25208);
#6853=VERTEX_POINT('',#25210);
#6854=VERTEX_POINT('',#25212);
#6855=VERTEX_POINT('',#25214);
#6856=VERTEX_POINT('',#25216);
#6857=VERTEX_POINT('',#25218);
#6858=VERTEX_POINT('',#25220);
#6859=VERTEX_POINT('',#25222);
#6860=VERTEX_POINT('',#25224);
#6861=VERTEX_POINT('',#25226);
#6862=VERTEX_POINT('',#25228);
#6863=VERTEX_POINT('',#25230);
#6864=VERTEX_POINT('',#25234);
#6865=VERTEX_POINT('',#25321);
#6866=VERTEX_POINT('',#25323);
#6867=VERTEX_POINT('',#25326);
#6868=VERTEX_POINT('',#25331);
#6869=VERTEX_POINT('',#25333);
#6870=VERTEX_POINT('',#25338);
#6871=VERTEX_POINT('',#25340);
#6872=VERTEX_POINT('',#25345);
#6873=VERTEX_POINT('',#25351);
#6874=VERTEX_POINT('',#25353);
#6875=VERTEX_POINT('',#25357);
#6876=VERTEX_POINT('',#25359);
#6877=VERTEX_POINT('',#25366);
#6878=VERTEX_POINT('',#25368);
#6879=VERTEX_POINT('',#25372);
#6880=VERTEX_POINT('',#25374);
#6881=VERTEX_POINT('',#25381);
#6882=VERTEX_POINT('',#25383);
#6883=VERTEX_POINT('',#25390);
#6884=VERTEX_POINT('',#25392);
#6885=VERTEX_POINT('',#25399);
#6886=VERTEX_POINT('',#25401);
#6887=VERTEX_POINT('',#25405);
#6888=VERTEX_POINT('',#25407);
#6889=VERTEX_POINT('',#25414);
#6890=VERTEX_POINT('',#25415);
#6891=VERTEX_POINT('',#25419);
#6892=VERTEX_POINT('',#25434);
#6893=VERTEX_POINT('',#25436);
#6894=VERTEX_POINT('',#25438);
#6895=VERTEX_POINT('',#25475);
#6896=VERTEX_POINT('',#25494);
#6897=VERTEX_POINT('',#25496);
#6898=VERTEX_POINT('',#25500);
#6899=VERTEX_POINT('',#25502);
#6900=VERTEX_POINT('',#25509);
#6901=VERTEX_POINT('',#25510);
#6902=VERTEX_POINT('',#25514);
#6903=VERTEX_POINT('',#25529);
#6904=VERTEX_POINT('',#25531);
#6905=VERTEX_POINT('',#25533);
#6906=VERTEX_POINT('',#25570);
#6907=VERTEX_POINT('',#25589);
#6908=VERTEX_POINT('',#25591);
#6909=VERTEX_POINT('',#25595);
#6910=VERTEX_POINT('',#25597);
#6911=VERTEX_POINT('',#25604);
#6912=VERTEX_POINT('',#25606);
#6913=VERTEX_POINT('',#25610);
#6914=VERTEX_POINT('',#25612);
#6915=VERTEX_POINT('',#25619);
#6916=VERTEX_POINT('',#25621);
#6917=VERTEX_POINT('',#25625);
#6918=VERTEX_POINT('',#25627);
#6919=VERTEX_POINT('',#25634);
#6920=VERTEX_POINT('',#25636);
#6921=VERTEX_POINT('',#25640);
#6922=VERTEX_POINT('',#25642);
#6923=VERTEX_POINT('',#25649);
#6924=VERTEX_POINT('',#25650);
#6925=VERTEX_POINT('',#25654);
#6926=VERTEX_POINT('',#25669);
#6927=VERTEX_POINT('',#25671);
#6928=VERTEX_POINT('',#25673);
#6929=VERTEX_POINT('',#25710);
#6930=VERTEX_POINT('',#25729);
#6931=VERTEX_POINT('',#25731);
#6932=VERTEX_POINT('',#25735);
#6933=VERTEX_POINT('',#25737);
#6934=VERTEX_POINT('',#25744);
#6935=VERTEX_POINT('',#25745);
#6936=VERTEX_POINT('',#25749);
#6937=VERTEX_POINT('',#25764);
#6938=VERTEX_POINT('',#25766);
#6939=VERTEX_POINT('',#25768);
#6940=VERTEX_POINT('',#25805);
#6941=VERTEX_POINT('',#25824);
#6942=VERTEX_POINT('',#25826);
#6943=VERTEX_POINT('',#25830);
#6944=VERTEX_POINT('',#25832);
#6945=VERTEX_POINT('',#25839);
#6946=VERTEX_POINT('',#25840);
#6947=VERTEX_POINT('',#25851);
#6948=VERTEX_POINT('',#25880);
#6949=VERTEX_POINT('',#25882);
#6950=VERTEX_POINT('',#25893);
#6951=VERTEX_POINT('',#25904);
#6952=VERTEX_POINT('',#25926);
#6953=VERTEX_POINT('',#25927);
#6954=VERTEX_POINT('',#25964);
#6955=VERTEX_POINT('',#25966);
#6956=VERTEX_POINT('',#25977);
#6957=VERTEX_POINT('',#26007);
#6958=VERTEX_POINT('',#26010);
#6959=VERTEX_POINT('',#26013);
#6960=VERTEX_POINT('',#26014);
#6961=VERTEX_POINT('',#26033);
#6962=VERTEX_POINT('',#26054);
#6963=VERTEX_POINT('',#26055);
#6964=VERTEX_POINT('',#26074);
#6965=VERTEX_POINT('',#26096);
#6966=VERTEX_POINT('',#26098);
#6967=VERTEX_POINT('',#26136);
#6968=VERTEX_POINT('',#26137);
#6969=VERTEX_POINT('',#26176);
#6970=VERTEX_POINT('',#26179);
#6971=VERTEX_POINT('',#26184);
#6972=VERTEX_POINT('',#26186);
#6973=VERTEX_POINT('',#26187);
#6974=VERTEX_POINT('',#26189);
#6975=VERTEX_POINT('',#26191);
#6976=VERTEX_POINT('',#26193);
#6977=VERTEX_POINT('',#26195);
#6978=VERTEX_POINT('',#26197);
#6979=VERTEX_POINT('',#26199);
#6980=VERTEX_POINT('',#26201);
#6981=VERTEX_POINT('',#26203);
#6982=VERTEX_POINT('',#26205);
#6983=VERTEX_POINT('',#26207);
#6984=VERTEX_POINT('',#26209);
#6985=VERTEX_POINT('',#26211);
#6986=VERTEX_POINT('',#26213);
#6987=VERTEX_POINT('',#26215);
#6988=VERTEX_POINT('',#26217);
#6989=VERTEX_POINT('',#26219);
#6990=VERTEX_POINT('',#26221);
#6991=VERTEX_POINT('',#26223);
#6992=VERTEX_POINT('',#26225);
#6993=VERTEX_POINT('',#26227);
#6994=VERTEX_POINT('',#26229);
#6995=VERTEX_POINT('',#26231);
#6996=VERTEX_POINT('',#26233);
#6997=VERTEX_POINT('',#26235);
#6998=VERTEX_POINT('',#26237);
#6999=VERTEX_POINT('',#26239);
#7000=VERTEX_POINT('',#26241);
#7001=VERTEX_POINT('',#26243);
#7002=VERTEX_POINT('',#26245);
#7003=VERTEX_POINT('',#26247);
#7004=VERTEX_POINT('',#26249);
#7005=VERTEX_POINT('',#26251);
#7006=VERTEX_POINT('',#26253);
#7007=VERTEX_POINT('',#26255);
#7008=VERTEX_POINT('',#26257);
#7009=VERTEX_POINT('',#26259);
#7010=VERTEX_POINT('',#26261);
#7011=VERTEX_POINT('',#26263);
#7012=VERTEX_POINT('',#26265);
#7013=VERTEX_POINT('',#26267);
#7014=VERTEX_POINT('',#26269);
#7015=VERTEX_POINT('',#26271);
#7016=VERTEX_POINT('',#26273);
#7017=VERTEX_POINT('',#26275);
#7018=VERTEX_POINT('',#26277);
#7019=VERTEX_POINT('',#26279);
#7020=VERTEX_POINT('',#26281);
#7021=VERTEX_POINT('',#26283);
#7022=VERTEX_POINT('',#26285);
#7023=VERTEX_POINT('',#26287);
#7024=VERTEX_POINT('',#26289);
#7025=VERTEX_POINT('',#26291);
#7026=VERTEX_POINT('',#26293);
#7027=VERTEX_POINT('',#26295);
#7028=VERTEX_POINT('',#26297);
#7029=VERTEX_POINT('',#26299);
#7030=VERTEX_POINT('',#26301);
#7031=VERTEX_POINT('',#26303);
#7032=VERTEX_POINT('',#26305);
#7033=VERTEX_POINT('',#26307);
#7034=VERTEX_POINT('',#26309);
#7035=VERTEX_POINT('',#26311);
#7036=VERTEX_POINT('',#26313);
#7037=VERTEX_POINT('',#26315);
#7038=VERTEX_POINT('',#26317);
#7039=VERTEX_POINT('',#26319);
#7040=VERTEX_POINT('',#26321);
#7041=VERTEX_POINT('',#26323);
#7042=VERTEX_POINT('',#26325);
#7043=VERTEX_POINT('',#26327);
#7044=VERTEX_POINT('',#26329);
#7045=VERTEX_POINT('',#26331);
#7046=VERTEX_POINT('',#26333);
#7047=VERTEX_POINT('',#26335);
#7048=VERTEX_POINT('',#26337);
#7049=VERTEX_POINT('',#26339);
#7050=VERTEX_POINT('',#26341);
#7051=VERTEX_POINT('',#26343);
#7052=VERTEX_POINT('',#26347);
#7053=VERTEX_POINT('',#26352);
#7054=VERTEX_POINT('',#26354);
#7055=VERTEX_POINT('',#26355);
#7056=VERTEX_POINT('',#26357);
#7057=VERTEX_POINT('',#26359);
#7058=VERTEX_POINT('',#26361);
#7059=VERTEX_POINT('',#26363);
#7060=VERTEX_POINT('',#26365);
#7061=VERTEX_POINT('',#26367);
#7062=VERTEX_POINT('',#26369);
#7063=VERTEX_POINT('',#26371);
#7064=VERTEX_POINT('',#26373);
#7065=VERTEX_POINT('',#26375);
#7066=VERTEX_POINT('',#26377);
#7067=VERTEX_POINT('',#26379);
#7068=VERTEX_POINT('',#26381);
#7069=VERTEX_POINT('',#26383);
#7070=VERTEX_POINT('',#26385);
#7071=VERTEX_POINT('',#26387);
#7072=VERTEX_POINT('',#26389);
#7073=VERTEX_POINT('',#26391);
#7074=VERTEX_POINT('',#26393);
#7075=VERTEX_POINT('',#26395);
#7076=VERTEX_POINT('',#26397);
#7077=VERTEX_POINT('',#26399);
#7078=VERTEX_POINT('',#26401);
#7079=VERTEX_POINT('',#26403);
#7080=VERTEX_POINT('',#26405);
#7081=VERTEX_POINT('',#26407);
#7082=VERTEX_POINT('',#26409);
#7083=VERTEX_POINT('',#26411);
#7084=VERTEX_POINT('',#26413);
#7085=VERTEX_POINT('',#26415);
#7086=VERTEX_POINT('',#26417);
#7087=VERTEX_POINT('',#26419);
#7088=VERTEX_POINT('',#26421);
#7089=VERTEX_POINT('',#26423);
#7090=VERTEX_POINT('',#26425);
#7091=VERTEX_POINT('',#26427);
#7092=VERTEX_POINT('',#26429);
#7093=VERTEX_POINT('',#26431);
#7094=VERTEX_POINT('',#26433);
#7095=VERTEX_POINT('',#26435);
#7096=VERTEX_POINT('',#26437);
#7097=VERTEX_POINT('',#26439);
#7098=VERTEX_POINT('',#26441);
#7099=VERTEX_POINT('',#26443);
#7100=VERTEX_POINT('',#26445);
#7101=VERTEX_POINT('',#26447);
#7102=VERTEX_POINT('',#26449);
#7103=VERTEX_POINT('',#26451);
#7104=VERTEX_POINT('',#26453);
#7105=VERTEX_POINT('',#26455);
#7106=VERTEX_POINT('',#26457);
#7107=VERTEX_POINT('',#26459);
#7108=VERTEX_POINT('',#26461);
#7109=VERTEX_POINT('',#26463);
#7110=VERTEX_POINT('',#26465);
#7111=VERTEX_POINT('',#26467);
#7112=VERTEX_POINT('',#26469);
#7113=VERTEX_POINT('',#26471);
#7114=VERTEX_POINT('',#26473);
#7115=VERTEX_POINT('',#26475);
#7116=VERTEX_POINT('',#26477);
#7117=VERTEX_POINT('',#26479);
#7118=VERTEX_POINT('',#26481);
#7119=VERTEX_POINT('',#26483);
#7120=VERTEX_POINT('',#26485);
#7121=VERTEX_POINT('',#26487);
#7122=VERTEX_POINT('',#26489);
#7123=VERTEX_POINT('',#26491);
#7124=VERTEX_POINT('',#26493);
#7125=VERTEX_POINT('',#26495);
#7126=VERTEX_POINT('',#26497);
#7127=VERTEX_POINT('',#26499);
#7128=VERTEX_POINT('',#26501);
#7129=VERTEX_POINT('',#26503);
#7130=VERTEX_POINT('',#26505);
#7131=VERTEX_POINT('',#26507);
#7132=VERTEX_POINT('',#26509);
#7133=VERTEX_POINT('',#26511);
#7134=VERTEX_POINT('',#26515);
#7135=VERTEX_POINT('',#26681);
#7136=VERTEX_POINT('',#26684);
#7137=VERTEX_POINT('',#26688);
#7138=VERTEX_POINT('',#26692);
#7139=VERTEX_POINT('',#26696);
#7140=VERTEX_POINT('',#26699);
#7141=VERTEX_POINT('',#26703);
#7142=VERTEX_POINT('',#26707);
#7143=VERTEX_POINT('',#26712);
#7144=VERTEX_POINT('',#26713);
#7145=VERTEX_POINT('',#26715);
#7146=VERTEX_POINT('',#26717);
#7147=VERTEX_POINT('',#26721);
#7148=VERTEX_POINT('',#26723);
#7149=VERTEX_POINT('',#26727);
#7150=VERTEX_POINT('',#26729);
#7151=VERTEX_POINT('',#26733);
#7152=VERTEX_POINT('',#26735);
#7153=VERTEX_POINT('',#26739);
#7154=VERTEX_POINT('',#26741);
#7155=VERTEX_POINT('',#26830);
#7156=VERTEX_POINT('',#26831);
#7157=VERTEX_POINT('',#26833);
#7158=VERTEX_POINT('',#26835);
#7159=VERTEX_POINT('',#26839);
#7160=VERTEX_POINT('',#26841);
#7161=VERTEX_POINT('',#26845);
#7162=VERTEX_POINT('',#26847);
#7163=VERTEX_POINT('',#26851);
#7164=VERTEX_POINT('',#26853);
#7165=VERTEX_POINT('',#26857);
#7166=VERTEX_POINT('',#26859);
#7167=VERTEX_POINT('',#26867);
#7168=VERTEX_POINT('',#26870);
#7169=VERTEX_POINT('',#26874);
#7170=VERTEX_POINT('',#26878);
#7171=EDGE_CURVE('',#5953,#5953,#5082,.T.);
#7172=EDGE_CURVE('',#5953,#5954,#3498,.T.);
#7173=EDGE_CURVE('',#5954,#5954,#5083,.T.);
#7174=EDGE_CURVE('',#5955,#5955,#5084,.T.);
#7175=EDGE_CURVE('',#5955,#5956,#3499,.T.);
#7176=EDGE_CURVE('',#5956,#5956,#5085,.T.);
#7177=EDGE_CURVE('',#5957,#5957,#5086,.T.);
#7178=EDGE_CURVE('',#5957,#5958,#3500,.T.);
#7179=EDGE_CURVE('',#5958,#5958,#5087,.T.);
#7180=EDGE_CURVE('',#5959,#5959,#5088,.T.);
#7181=EDGE_CURVE('',#5959,#5960,#3501,.T.);
#7182=EDGE_CURVE('',#5960,#5960,#5089,.T.);
#7183=EDGE_CURVE('',#5961,#5961,#5090,.T.);
#7184=EDGE_CURVE('',#5961,#5962,#3502,.T.);
#7185=EDGE_CURVE('',#5962,#5962,#5091,.T.);
#7186=EDGE_CURVE('',#5963,#5963,#5092,.T.);
#7187=EDGE_CURVE('',#5963,#5964,#3503,.T.);
#7188=EDGE_CURVE('',#5964,#5964,#5093,.T.);
#7189=EDGE_CURVE('',#5965,#5965,#5094,.T.);
#7190=EDGE_CURVE('',#5965,#5966,#3504,.T.);
#7191=EDGE_CURVE('',#5966,#5966,#5095,.T.);
#7192=EDGE_CURVE('',#5967,#5967,#5096,.T.);
#7193=EDGE_CURVE('',#5967,#5968,#3505,.T.);
#7194=EDGE_CURVE('',#5968,#5968,#5097,.T.);
#7195=EDGE_CURVE('',#5969,#5969,#5098,.T.);
#7196=EDGE_CURVE('',#5969,#5970,#3506,.T.);
#7197=EDGE_CURVE('',#5970,#5970,#5099,.T.);
#7198=EDGE_CURVE('',#5971,#5971,#5100,.T.);
#7199=EDGE_CURVE('',#5971,#5972,#3507,.T.);
#7200=EDGE_CURVE('',#5972,#5972,#5101,.T.);
#7201=EDGE_CURVE('',#5973,#5974,#3508,.T.);
#7202=EDGE_CURVE('',#5975,#5973,#5102,.T.);
#7203=EDGE_CURVE('',#5975,#5976,#3509,.T.);
#7204=EDGE_CURVE('',#5974,#5976,#5103,.T.);
#7205=EDGE_CURVE('',#5977,#5978,#3510,.T.);
#7206=EDGE_CURVE('',#5979,#5978,#5104,.T.);
#7207=EDGE_CURVE('',#5980,#5979,#3511,.T.);
#7208=EDGE_CURVE('',#5977,#5980,#5105,.T.);
#7209=EDGE_CURVE('',#5981,#5982,#3512,.T.);
#7210=EDGE_CURVE('',#5983,#5981,#3513,.T.);
#7211=EDGE_CURVE('',#5984,#5983,#3514,.T.);
#7212=EDGE_CURVE('',#5982,#5984,#3515,.T.);
#7213=EDGE_CURVE('',#5985,#5986,#5106,.T.);
#7214=EDGE_CURVE('',#5986,#5987,#3516,.T.);
#7215=EDGE_CURVE('',#5987,#5988,#5107,.T.);
#7216=EDGE_CURVE('',#5988,#5985,#3517,.T.);
#7217=EDGE_CURVE('',#5989,#5990,#5108,.T.);
#7218=EDGE_CURVE('',#5990,#5991,#3518,.T.);
#7219=EDGE_CURVE('',#5991,#5992,#5109,.T.);
#7220=EDGE_CURVE('',#5992,#5989,#3519,.T.);
#7221=EDGE_CURVE('',#5993,#5994,#5110,.T.);
#7222=EDGE_CURVE('',#5994,#5995,#3520,.T.);
#7223=EDGE_CURVE('',#5995,#5996,#5111,.T.);
#7224=EDGE_CURVE('',#5996,#5993,#3521,.T.);
#7225=EDGE_CURVE('',#5973,#5977,#3522,.T.);
#7226=EDGE_CURVE('',#5980,#5975,#3523,.T.);
#7227=EDGE_CURVE('',#5976,#5979,#3524,.T.);
#7228=EDGE_CURVE('',#5978,#5974,#3525,.T.);
#7229=EDGE_CURVE('',#5986,#5997,#3526,.T.);
#7230=EDGE_CURVE('',#5985,#5998,#3527,.T.);
#7231=EDGE_CURVE('',#5997,#5998,#5112,.T.);
#7232=EDGE_CURVE('',#5987,#5999,#3528,.T.);
#7233=EDGE_CURVE('',#6000,#5999,#5113,.T.);
#7234=EDGE_CURVE('',#5988,#6000,#3529,.T.);
#7235=EDGE_CURVE('',#5998,#6000,#3530,.T.);
#7236=EDGE_CURVE('',#5999,#5997,#3531,.T.);
#7237=EDGE_CURVE('',#6001,#6002,#3532,.T.);
#7238=EDGE_CURVE('',#6003,#6001,#5114,.T.);
#7239=EDGE_CURVE('',#5994,#6003,#3533,.T.);
#7240=EDGE_CURVE('',#5993,#6004,#3534,.T.);
#7241=EDGE_CURVE('',#6005,#6004,#5115,.T.);
#7242=EDGE_CURVE('',#6006,#6005,#3535,.T.);
#7243=EDGE_CURVE('',#6002,#6006,#5116,.T.);
#7244=EDGE_CURVE('',#5995,#6007,#3536,.T.);
#7245=EDGE_CURVE('',#6008,#6007,#5117,.T.);
#7246=EDGE_CURVE('',#5996,#6008,#3537,.T.);
#7247=EDGE_CURVE('',#6004,#6008,#3538,.T.);
#7248=EDGE_CURVE('',#6007,#6003,#3539,.T.);
#7249=EDGE_CURVE('',#6009,#6010,#3540,.T.);
#7250=EDGE_CURVE('',#6011,#6009,#5118,.T.);
#7251=EDGE_CURVE('',#5990,#6011,#3541,.T.);
#7252=EDGE_CURVE('',#5989,#6012,#3542,.T.);
#7253=EDGE_CURVE('',#6013,#6012,#5119,.T.);
#7254=EDGE_CURVE('',#6014,#6013,#3543,.T.);
#7255=EDGE_CURVE('',#6010,#6014,#5120,.T.);
#7256=EDGE_CURVE('',#5991,#6015,#3544,.T.);
#7257=EDGE_CURVE('',#6016,#6015,#5121,.T.);
#7258=EDGE_CURVE('',#5992,#6016,#3545,.T.);
#7259=EDGE_CURVE('',#6012,#6016,#3546,.T.);
#7260=EDGE_CURVE('',#6015,#6011,#3547,.T.);
#7261=EDGE_CURVE('',#6009,#6013,#5122,.T.);
#7262=EDGE_CURVE('',#6014,#6010,#5123,.T.);
#7263=EDGE_CURVE('',#6017,#6017,#5124,.T.);
#7264=EDGE_CURVE('',#6017,#6018,#3548,.T.);
#7265=EDGE_CURVE('',#6018,#6018,#5125,.T.);
#7266=EDGE_CURVE('',#6019,#6019,#5126,.T.);
#7267=EDGE_CURVE('',#6019,#6020,#3549,.T.);
#7268=EDGE_CURVE('',#6020,#6020,#5127,.T.);
#7269=EDGE_CURVE('',#6001,#6005,#5128,.T.);
#7270=EDGE_CURVE('',#6006,#6002,#5129,.T.);
#7271=EDGE_CURVE('',#5981,#6021,#3550,.T.);
#7272=EDGE_CURVE('',#6022,#6021,#3551,.T.);
#7273=EDGE_CURVE('',#5983,#6022,#3552,.T.);
#7274=EDGE_CURVE('',#6023,#6022,#3553,.T.);
#7275=EDGE_CURVE('',#5984,#6023,#3554,.T.);
#7276=EDGE_CURVE('',#6024,#6023,#3555,.T.);
#7277=EDGE_CURVE('',#5982,#6024,#3556,.T.);
#7278=EDGE_CURVE('',#6021,#6024,#3557,.T.);
#7279=EDGE_CURVE('',#6025,#6026,#3558,.T.);
#7280=EDGE_CURVE('',#6026,#6027,#3559,.T.);
#7281=EDGE_CURVE('',#6028,#6027,#3560,.T.);
#7282=EDGE_CURVE('',#6025,#6028,#3561,.T.);
#7283=EDGE_CURVE('',#6029,#6025,#3562,.T.);
#7284=EDGE_CURVE('',#6030,#6028,#3563,.T.);
#7285=EDGE_CURVE('',#6029,#6030,#3564,.T.);
#7286=EDGE_CURVE('',#6031,#6029,#3565,.T.);
#7287=EDGE_CURVE('',#6032,#6030,#3566,.T.);
#7288=EDGE_CURVE('',#6031,#6032,#3567,.T.);
#7289=EDGE_CURVE('',#6026,#6031,#3568,.T.);
#7290=EDGE_CURVE('',#6027,#6032,#3569,.T.);
#7291=EDGE_CURVE('',#6033,#6034,#3570,.T.);
#7292=EDGE_CURVE('',#6034,#6035,#3571,.T.);
#7293=EDGE_CURVE('',#6036,#6035,#3572,.T.);
#7294=EDGE_CURVE('',#6033,#6036,#3573,.T.);
#7295=EDGE_CURVE('',#6037,#6033,#3574,.T.);
#7296=EDGE_CURVE('',#6038,#6036,#3575,.T.);
#7297=EDGE_CURVE('',#6037,#6038,#3576,.T.);
#7298=EDGE_CURVE('',#6039,#6037,#3577,.T.);
#7299=EDGE_CURVE('',#6040,#6038,#3578,.T.);
#7300=EDGE_CURVE('',#6039,#6040,#3579,.T.);
#7301=EDGE_CURVE('',#6034,#6039,#3580,.T.);
#7302=EDGE_CURVE('',#6035,#6040,#3581,.T.);
#7303=EDGE_CURVE('',#6041,#6041,#5130,.T.);
#7304=EDGE_CURVE('',#6041,#6042,#3582,.T.);
#7305=EDGE_CURVE('',#6042,#6042,#5131,.T.);
#7306=EDGE_CURVE('',#6043,#6043,#5132,.T.);
#7307=EDGE_CURVE('',#6043,#6044,#3583,.T.);
#7308=EDGE_CURVE('',#6044,#6044,#5133,.T.);
#7309=EDGE_CURVE('',#6045,#6045,#5134,.T.);
#7310=EDGE_CURVE('',#6045,#6046,#3584,.T.);
#7311=EDGE_CURVE('',#6046,#6046,#5135,.T.);
#7312=EDGE_CURVE('',#6047,#6047,#5136,.T.);
#7313=EDGE_CURVE('',#6047,#6048,#3585,.T.);
#7314=EDGE_CURVE('',#6048,#6048,#5137,.T.);
#7315=EDGE_CURVE('',#6049,#6049,#5138,.T.);
#7316=EDGE_CURVE('',#6049,#6050,#3586,.T.);
#7317=EDGE_CURVE('',#6050,#6050,#5139,.T.);
#7318=EDGE_CURVE('',#6051,#6051,#5140,.T.);
#7319=EDGE_CURVE('',#6051,#6052,#3587,.T.);
#7320=EDGE_CURVE('',#6052,#6052,#5141,.T.);
#7321=EDGE_CURVE('',#6053,#6053,#5142,.T.);
#7322=EDGE_CURVE('',#6053,#6054,#3588,.T.);
#7323=EDGE_CURVE('',#6054,#6054,#5143,.T.);
#7324=EDGE_CURVE('',#6055,#6055,#5144,.T.);
#7325=EDGE_CURVE('',#6055,#6056,#3589,.T.);
#7326=EDGE_CURVE('',#6056,#6056,#5145,.T.);
#7327=EDGE_CURVE('',#6057,#6057,#5146,.T.);
#7328=EDGE_CURVE('',#6057,#6058,#3590,.T.);
#7329=EDGE_CURVE('',#6058,#6058,#5147,.T.);
#7330=EDGE_CURVE('',#6059,#6060,#3591,.T.);
#7331=EDGE_CURVE('',#6061,#6059,#3592,.T.);
#7332=EDGE_CURVE('',#6061,#6062,#3593,.T.);
#7333=EDGE_CURVE('',#6060,#6062,#3594,.T.);
#7334=EDGE_CURVE('',#6063,#6064,#3595,.T.);
#7335=EDGE_CURVE('',#6065,#6063,#3596,.T.);
#7336=EDGE_CURVE('',#6066,#6065,#3597,.T.);
#7337=EDGE_CURVE('',#6064,#6066,#3598,.T.);
#7338=EDGE_CURVE('',#6066,#6067,#3599,.T.);
#7339=EDGE_CURVE('',#6068,#6065,#3600,.T.);
#7340=EDGE_CURVE('',#6067,#6068,#3601,.T.);
#7341=EDGE_CURVE('',#6069,#6061,#3602,.T.);
#7342=EDGE_CURVE('',#6069,#6070,#3603,.T.);
#7343=EDGE_CURVE('',#6062,#6070,#3604,.T.);
#7344=EDGE_CURVE('',#6059,#6071,#3605,.T.);
#7345=EDGE_CURVE('',#6072,#6071,#3606,.T.);
#7346=EDGE_CURVE('',#6064,#6072,#3607,.T.);
#7347=EDGE_CURVE('',#6067,#6069,#3608,.T.);
#7348=EDGE_CURVE('',#6060,#6073,#3609,.T.);
#7349=EDGE_CURVE('',#6071,#6073,#3610,.T.);
#7350=EDGE_CURVE('',#6063,#6074,#3611,.T.);
#7351=EDGE_CURVE('',#6073,#6074,#3612,.T.);
#7352=EDGE_CURVE('',#6070,#6068,#3613,.T.);
#7353=EDGE_CURVE('',#6074,#6072,#3614,.T.);
#7354=EDGE_CURVE('',#6075,#6075,#5148,.T.);
#7355=EDGE_CURVE('',#6075,#6076,#3615,.T.);
#7356=EDGE_CURVE('',#6076,#6076,#5149,.T.);
#7357=EDGE_CURVE('',#6077,#6077,#5150,.T.);
#7358=EDGE_CURVE('',#6077,#6078,#3616,.T.);
#7359=EDGE_CURVE('',#6078,#6078,#5151,.T.);
#7360=EDGE_CURVE('',#6079,#6080,#3617,.T.);
#7361=EDGE_CURVE('',#6081,#6079,#5152,.T.);
#7362=EDGE_CURVE('',#6082,#6081,#3618,.T.);
#7363=EDGE_CURVE('',#6080,#6082,#5153,.T.);
#7364=EDGE_CURVE('',#6083,#6084,#3619,.T.);
#7365=EDGE_CURVE('',#6085,#6083,#5154,.T.);
#7366=EDGE_CURVE('',#6086,#6085,#3620,.T.);
#7367=EDGE_CURVE('',#6084,#6086,#5155,.T.);
#7368=EDGE_CURVE('',#6087,#6088,#3621,.T.);
#7369=EDGE_CURVE('',#6089,#6087,#5156,.T.);
#7370=EDGE_CURVE('',#6090,#6089,#3622,.T.);
#7371=EDGE_CURVE('',#6088,#6090,#5157,.T.);
#7372=EDGE_CURVE('',#6091,#6092,#3623,.T.);
#7373=EDGE_CURVE('',#6093,#6091,#5158,.T.);
#7374=EDGE_CURVE('',#6094,#6093,#3624,.T.);
#7375=EDGE_CURVE('',#6092,#6094,#5159,.T.);
#7376=EDGE_CURVE('',#6093,#6079,#5160,.T.);
#7377=EDGE_CURVE('',#6089,#6091,#5161,.T.);
#7378=EDGE_CURVE('',#6085,#6087,#5162,.T.);
#7379=EDGE_CURVE('',#6081,#6083,#5163,.T.);
#7380=EDGE_CURVE('',#6095,#6095,#5164,.T.);
#7381=EDGE_CURVE('',#6090,#6092,#5165,.T.);
#7382=EDGE_CURVE('',#6086,#6088,#5166,.T.);
#7383=EDGE_CURVE('',#6094,#6080,#5167,.T.);
#7384=EDGE_CURVE('',#6082,#6084,#5168,.T.);
#7385=EDGE_CURVE('',#6096,#6096,#5169,.T.);
#7386=EDGE_CURVE('',#6096,#6097,#3625,.T.);
#7387=EDGE_CURVE('',#6097,#6097,#5170,.T.);
#7388=EDGE_CURVE('',#6098,#6098,#5171,.T.);
#7389=EDGE_CURVE('',#6098,#6095,#3626,.T.);
#7390=EDGE_CURVE('',#6099,#6100,#3627,.T.);
#7391=EDGE_CURVE('',#6101,#6099,#5172,.T.);
#7392=EDGE_CURVE('',#6102,#6101,#3628,.T.);
#7393=EDGE_CURVE('',#6100,#6102,#5173,.T.);
#7394=EDGE_CURVE('',#6103,#6104,#3629,.T.);
#7395=EDGE_CURVE('',#6105,#6103,#5174,.T.);
#7396=EDGE_CURVE('',#6106,#6105,#3630,.T.);
#7397=EDGE_CURVE('',#6104,#6106,#5175,.T.);
#7398=EDGE_CURVE('',#6107,#6108,#3631,.T.);
#7399=EDGE_CURVE('',#6109,#6107,#5176,.T.);
#7400=EDGE_CURVE('',#6110,#6109,#3632,.T.);
#7401=EDGE_CURVE('',#6108,#6110,#5177,.T.);
#7402=EDGE_CURVE('',#6111,#6112,#3633,.T.);
#7403=EDGE_CURVE('',#6113,#6111,#5178,.T.);
#7404=EDGE_CURVE('',#6114,#6113,#3634,.T.);
#7405=EDGE_CURVE('',#6112,#6114,#5179,.T.);
#7406=EDGE_CURVE('',#6113,#6099,#5180,.T.);
#7407=EDGE_CURVE('',#6109,#6111,#5181,.T.);
#7408=EDGE_CURVE('',#6105,#6107,#5182,.T.);
#7409=EDGE_CURVE('',#6101,#6103,#5183,.T.);
#7410=EDGE_CURVE('',#6115,#6115,#5184,.T.);
#7411=EDGE_CURVE('',#6110,#6112,#5185,.T.);
#7412=EDGE_CURVE('',#6106,#6108,#5186,.T.);
#7413=EDGE_CURVE('',#6114,#6100,#5187,.T.);
#7414=EDGE_CURVE('',#6102,#6104,#5188,.T.);
#7415=EDGE_CURVE('',#6115,#6116,#3635,.T.);
#7416=EDGE_CURVE('',#6116,#6116,#5189,.T.);
#7417=EDGE_CURVE('',#6117,#6117,#5190,.T.);
#7418=EDGE_CURVE('',#6118,#6118,#5191,.T.);
#7419=EDGE_CURVE('',#6118,#6117,#3636,.T.);
#7420=EDGE_CURVE('',#6119,#6120,#3637,.T.);
#7421=EDGE_CURVE('',#6121,#6119,#5192,.T.);
#7422=EDGE_CURVE('',#6122,#6121,#3638,.T.);
#7423=EDGE_CURVE('',#6120,#6122,#5193,.T.);
#7424=EDGE_CURVE('',#6123,#6124,#3639,.T.);
#7425=EDGE_CURVE('',#6125,#6123,#5194,.T.);
#7426=EDGE_CURVE('',#6126,#6125,#3640,.T.);
#7427=EDGE_CURVE('',#6124,#6126,#5195,.T.);
#7428=EDGE_CURVE('',#6127,#6119,#3641,.T.);
#7429=EDGE_CURVE('',#6127,#6128,#5196,.T.);
#7430=EDGE_CURVE('',#6124,#6128,#3642,.T.);
#7431=EDGE_CURVE('',#6121,#6126,#3643,.T.);
#7432=EDGE_CURVE('',#6129,#6129,#5197,.T.);
#7433=EDGE_CURVE('',#6130,#6130,#5198,.T.);
#7434=EDGE_CURVE('',#6131,#6131,#5199,.T.);
#7435=EDGE_CURVE('',#6132,#6132,#5200,.T.);
#7436=EDGE_CURVE('',#6133,#6133,#5201,.T.);
#7437=EDGE_CURVE('',#6134,#6127,#3644,.T.);
#7438=EDGE_CURVE('',#6135,#6134,#5202,.T.);
#7439=EDGE_CURVE('',#6128,#6135,#3645,.T.);
#7440=EDGE_CURVE('',#6120,#6136,#3646,.T.);
#7441=EDGE_CURVE('',#6137,#6136,#3647,.T.);
#7442=EDGE_CURVE('',#6138,#6137,#3648,.T.);
#7443=EDGE_CURVE('',#6138,#6139,#3649,.T.);
#7444=EDGE_CURVE('',#6139,#6134,#3650,.T.);
#7445=EDGE_CURVE('',#6125,#6140,#3651,.T.);
#7446=EDGE_CURVE('',#6140,#6141,#3652,.T.);
#7447=EDGE_CURVE('',#6141,#6137,#3653,.T.);
#7448=EDGE_CURVE('',#6136,#6122,#3654,.T.);
#7449=EDGE_CURVE('',#6123,#6140,#3655,.T.);
#7450=EDGE_CURVE('',#6142,#6142,#5203,.T.);
#7451=EDGE_CURVE('',#6142,#6133,#3656,.T.);
#7452=EDGE_CURVE('',#6143,#6143,#5204,.T.);
#7453=EDGE_CURVE('',#6143,#6132,#3657,.T.);
#7454=EDGE_CURVE('',#6144,#6144,#5205,.T.);
#7455=EDGE_CURVE('',#6144,#6131,#3658,.T.);
#7456=EDGE_CURVE('',#6145,#6145,#5206,.T.);
#7457=EDGE_CURVE('',#6145,#6130,#3659,.T.);
#7458=EDGE_CURVE('',#6146,#6146,#5207,.T.);
#7459=EDGE_CURVE('',#6146,#6129,#3660,.T.);
#7460=EDGE_CURVE('',#6147,#6147,#5208,.T.);
#7461=EDGE_CURVE('',#6147,#6148,#3661,.T.);
#7462=EDGE_CURVE('',#6148,#6148,#5209,.T.);
#7463=EDGE_CURVE('',#6149,#6149,#5210,.T.);
#7464=EDGE_CURVE('',#6149,#6150,#3662,.T.);
#7465=EDGE_CURVE('',#6150,#6150,#5211,.T.);
#7466=EDGE_CURVE('',#6151,#6151,#5212,.T.);
#7467=EDGE_CURVE('',#6151,#6152,#3663,.T.);
#7468=EDGE_CURVE('',#6152,#6152,#5213,.T.);
#7469=EDGE_CURVE('',#6153,#6153,#5214,.T.);
#7470=EDGE_CURVE('',#6153,#6154,#3664,.T.);
#7471=EDGE_CURVE('',#6154,#6154,#5215,.T.);
#7472=EDGE_CURVE('',#6155,#6138,#3665,.T.);
#7473=EDGE_CURVE('',#6155,#6156,#3666,.T.);
#7474=EDGE_CURVE('',#6139,#6156,#3667,.T.);
#7475=EDGE_CURVE('',#6157,#6158,#3668,.T.);
#7476=EDGE_CURVE('',#6159,#6157,#3669,.T.);
#7477=EDGE_CURVE('',#6160,#6159,#3670,.T.);
#7478=EDGE_CURVE('',#6158,#6160,#3671,.T.);
#7479=EDGE_CURVE('',#6160,#6161,#3672,.T.);
#7480=EDGE_CURVE('',#6162,#6159,#3673,.T.);
#7481=EDGE_CURVE('',#6161,#6162,#3674,.T.);
#7482=EDGE_CURVE('',#6163,#6155,#3675,.T.);
#7483=EDGE_CURVE('',#6163,#6164,#3676,.T.);
#7484=EDGE_CURVE('',#6156,#6164,#3677,.T.);
#7485=EDGE_CURVE('',#6158,#6141,#3678,.T.);
#7486=EDGE_CURVE('',#6161,#6163,#3679,.T.);
#7487=EDGE_CURVE('',#6164,#6162,#3680,.T.);
#7488=EDGE_CURVE('',#6157,#6135,#3681,.T.);
#7489=EDGE_CURVE('',#6165,#6165,#5216,.T.);
#7490=EDGE_CURVE('',#6165,#6166,#3682,.T.);
#7491=EDGE_CURVE('',#6166,#6166,#5217,.T.);
#7492=EDGE_CURVE('',#6167,#6167,#5218,.T.);
#7493=EDGE_CURVE('',#6167,#6168,#3683,.T.);
#7494=EDGE_CURVE('',#6168,#6168,#5219,.T.);
#7495=EDGE_CURVE('',#6169,#6169,#5220,.T.);
#7496=EDGE_CURVE('',#6169,#6170,#3684,.T.);
#7497=EDGE_CURVE('',#6170,#6170,#5221,.T.);
#7498=EDGE_CURVE('',#6171,#6171,#5222,.T.);
#7499=EDGE_CURVE('',#6171,#6172,#3685,.T.);
#7500=EDGE_CURVE('',#6172,#6172,#5223,.T.);
#7501=EDGE_CURVE('',#6173,#6173,#5224,.T.);
#7502=EDGE_CURVE('',#6173,#6174,#3686,.T.);
#7503=EDGE_CURVE('',#6174,#6174,#5225,.T.);
#7504=EDGE_CURVE('',#6175,#6175,#5226,.T.);
#7505=EDGE_CURVE('',#6175,#6176,#3687,.T.);
#7506=EDGE_CURVE('',#6176,#6176,#5227,.T.);
#7507=EDGE_CURVE('',#6177,#6177,#5228,.T.);
#7508=EDGE_CURVE('',#6177,#6178,#3688,.T.);
#7509=EDGE_CURVE('',#6178,#6178,#5229,.T.);
#7510=EDGE_CURVE('',#6179,#6179,#5230,.T.);
#7511=EDGE_CURVE('',#6179,#6180,#3689,.T.);
#7512=EDGE_CURVE('',#6180,#6180,#5231,.T.);
#7513=EDGE_CURVE('',#6181,#6181,#5232,.T.);
#7514=EDGE_CURVE('',#6181,#6182,#3690,.T.);
#7515=EDGE_CURVE('',#6182,#6182,#5233,.T.);
#7516=EDGE_CURVE('',#6183,#6183,#5234,.T.);
#7517=EDGE_CURVE('',#6183,#6184,#3691,.T.);
#7518=EDGE_CURVE('',#6184,#6184,#5235,.T.);
#7519=EDGE_CURVE('',#6185,#6186,#3692,.T.);
#7520=EDGE_CURVE('',#6187,#6185,#5236,.T.);
#7521=EDGE_CURVE('',#6188,#6187,#3693,.T.);
#7522=EDGE_CURVE('',#6186,#6188,#5237,.T.);
#7523=EDGE_CURVE('',#6189,#6190,#3694,.T.);
#7524=EDGE_CURVE('',#6191,#6189,#5238,.T.);
#7525=EDGE_CURVE('',#6192,#6191,#3695,.T.);
#7526=EDGE_CURVE('',#6190,#6192,#5239,.T.);
#7527=EDGE_CURVE('',#6193,#6194,#3696,.T.);
#7528=EDGE_CURVE('',#6195,#6193,#5240,.T.);
#7529=EDGE_CURVE('',#6196,#6195,#3697,.T.);
#7530=EDGE_CURVE('',#6194,#6196,#5241,.T.);
#7531=EDGE_CURVE('',#6197,#6198,#3698,.T.);
#7532=EDGE_CURVE('',#6199,#6197,#5242,.T.);
#7533=EDGE_CURVE('',#6200,#6199,#3699,.T.);
#7534=EDGE_CURVE('',#6198,#6200,#5243,.T.);
#7535=EDGE_CURVE('',#6199,#6185,#5244,.T.);
#7536=EDGE_CURVE('',#6195,#6197,#5245,.T.);
#7537=EDGE_CURVE('',#6191,#6193,#5246,.T.);
#7538=EDGE_CURVE('',#6187,#6189,#5247,.T.);
#7539=EDGE_CURVE('',#6201,#6201,#5248,.T.);
#7540=EDGE_CURVE('',#6196,#6198,#5249,.T.);
#7541=EDGE_CURVE('',#6192,#6194,#5250,.T.);
#7542=EDGE_CURVE('',#6200,#6186,#5251,.T.);
#7543=EDGE_CURVE('',#6188,#6190,#5252,.T.);
#7544=EDGE_CURVE('',#6202,#6202,#5253,.T.);
#7545=EDGE_CURVE('',#6202,#6203,#3700,.T.);
#7546=EDGE_CURVE('',#6203,#6203,#5254,.T.);
#7547=EDGE_CURVE('',#6204,#6204,#5255,.T.);
#7548=EDGE_CURVE('',#6204,#6201,#3701,.T.);
#7549=EDGE_CURVE('',#6205,#6206,#3702,.T.);
#7550=EDGE_CURVE('',#6207,#6205,#5256,.T.);
#7551=EDGE_CURVE('',#6208,#6207,#3703,.T.);
#7552=EDGE_CURVE('',#6206,#6208,#5257,.T.);
#7553=EDGE_CURVE('',#6209,#6205,#5258,.T.);
#7554=EDGE_CURVE('',#6210,#6209,#5259,.T.);
#7555=EDGE_CURVE('',#6207,#6210,#5260,.T.);
#7556=EDGE_CURVE('',#6211,#6212,#5261,.T.);
#7557=EDGE_CURVE('',#6211,#6213,#5262,.T.);
#7558=EDGE_CURVE('',#6214,#6213,#5263,.T.);
#7559=EDGE_CURVE('',#6212,#6214,#5264,.T.);
#7560=EDGE_CURVE('',#6215,#6211,#3704,.T.);
#7561=EDGE_CURVE('',#6216,#6215,#5265,.T.);
#7562=EDGE_CURVE('',#6213,#6216,#3705,.T.);
#7563=EDGE_CURVE('',#6217,#6218,#5266,.T.);
#7564=EDGE_CURVE('',#6217,#6219,#5267,.T.);
#7565=EDGE_CURVE('',#6220,#6219,#5268,.T.);
#7566=EDGE_CURVE('',#6218,#6220,#5269,.T.);
#7567=EDGE_CURVE('',#6221,#6217,#3706,.T.);
#7568=EDGE_CURVE('',#6222,#6221,#5270,.T.);
#7569=EDGE_CURVE('',#6219,#6222,#3707,.T.);
#7570=EDGE_CURVE('',#6223,#6224,#5271,.T.);
#7571=EDGE_CURVE('',#6223,#6225,#5272,.T.);
#7572=EDGE_CURVE('',#6226,#6225,#5273,.T.);
#7573=EDGE_CURVE('',#6224,#6226,#5274,.T.);
#7574=EDGE_CURVE('',#6227,#6223,#3708,.T.);
#7575=EDGE_CURVE('',#6228,#6227,#5275,.T.);
#7576=EDGE_CURVE('',#6225,#6228,#3709,.T.);
#7577=EDGE_CURVE('',#6229,#6214,#3710,.T.);
#7578=EDGE_CURVE('',#6230,#6229,#5276,.T.);
#7579=EDGE_CURVE('',#6212,#6230,#3711,.T.);
#7580=EDGE_CURVE('',#6231,#6220,#3712,.T.);
#7581=EDGE_CURVE('',#6232,#6231,#5277,.T.);
#7582=EDGE_CURVE('',#6218,#6232,#3713,.T.);
#7583=EDGE_CURVE('',#6233,#6226,#3714,.T.);
#7584=EDGE_CURVE('',#6234,#6233,#5278,.T.);
#7585=EDGE_CURVE('',#6224,#6234,#3715,.T.);
#7586=EDGE_CURVE('',#6227,#6206,#5279,.T.);
#7587=EDGE_CURVE('',#6234,#6235,#5280,.T.);
#7588=EDGE_CURVE('',#6235,#6209,#3716,.T.);
#7589=EDGE_CURVE('',#6208,#6216,#5281,.T.);
#7590=EDGE_CURVE('',#6215,#6222,#5282,.T.);
#7591=EDGE_CURVE('',#6221,#6228,#5283,.T.);
#7592=EDGE_CURVE('',#6236,#6236,#5284,.T.);
#7593=EDGE_CURVE('',#6237,#6235,#5285,.T.);
#7594=EDGE_CURVE('',#6232,#6233,#5286,.T.);
#7595=EDGE_CURVE('',#6230,#6231,#5287,.T.);
#7596=EDGE_CURVE('',#6237,#6229,#5288,.T.);
#7597=EDGE_CURVE('',#6238,#6238,#5289,.T.);
#7598=EDGE_CURVE('',#6210,#6237,#3717,.T.);
#7599=EDGE_CURVE('',#6236,#6238,#3718,.T.);
#7600=EDGE_CURVE('',#6239,#6240,#3719,.T.);
#7601=EDGE_CURVE('',#6241,#6239,#3720,.T.);
#7602=EDGE_CURVE('',#6242,#6241,#3721,.T.);
#7603=EDGE_CURVE('',#6242,#6240,#3722,.T.);
#7604=EDGE_CURVE('',#6243,#6244,#3723,.T.);
#7605=EDGE_CURVE('',#6245,#6243,#3724,.T.);
#7606=EDGE_CURVE('',#6246,#6245,#3725,.T.);
#7607=EDGE_CURVE('',#6244,#6246,#3726,.T.);
#7608=EDGE_CURVE('',#6247,#6248,#3727,.T.);
#7609=EDGE_CURVE('',#6249,#6247,#5290,.T.);
#7610=EDGE_CURVE('',#6250,#6249,#3728,.T.);
#7611=EDGE_CURVE('',#6248,#6250,#5291,.T.);
#7612=EDGE_CURVE('',#6240,#6243,#5292,.T.);
#7613=EDGE_CURVE('',#6244,#6239,#5293,.T.);
#7614=EDGE_CURVE('',#6245,#6242,#5294,.T.);
#7615=EDGE_CURVE('',#6241,#6246,#5295,.T.);
#7616=EDGE_CURVE('',#6250,#6251,#3729,.T.);
#7617=EDGE_CURVE('',#6252,#6251,#5296,.T.);
#7618=EDGE_CURVE('',#6248,#6252,#3730,.T.);
#7619=EDGE_CURVE('',#6249,#6253,#3731,.T.);
#7620=EDGE_CURVE('',#6251,#6253,#3732,.T.);
#7621=EDGE_CURVE('',#6254,#6252,#3733,.T.);
#7622=EDGE_CURVE('',#6247,#6254,#3734,.T.);
#7623=EDGE_CURVE('',#6253,#6254,#5297,.T.);
#7624=EDGE_CURVE('',#6255,#6255,#5298,.T.);
#7625=EDGE_CURVE('',#6255,#6256,#3735,.T.);
#7626=EDGE_CURVE('',#6256,#6256,#5299,.T.);
#7627=EDGE_CURVE('',#6257,#6257,#5300,.T.);
#7628=EDGE_CURVE('',#6258,#6258,#5301,.T.);
#7629=EDGE_CURVE('',#6258,#6257,#3736,.T.);
#7630=EDGE_CURVE('',#6259,#6259,#5302,.T.);
#7631=EDGE_CURVE('',#6259,#6260,#3737,.T.);
#7632=EDGE_CURVE('',#6260,#6260,#5303,.T.);
#7633=EDGE_CURVE('',#6261,#6261,#5304,.T.);
#7634=EDGE_CURVE('',#6262,#6262,#5305,.T.);
#7635=EDGE_CURVE('',#6262,#6261,#3738,.T.);
#7636=EDGE_CURVE('',#6263,#6263,#5306,.T.);
#7637=EDGE_CURVE('',#6263,#6264,#3739,.T.);
#7638=EDGE_CURVE('',#6264,#6264,#5307,.T.);
#7639=EDGE_CURVE('',#6265,#6265,#5308,.T.);
#7640=EDGE_CURVE('',#6266,#6266,#5309,.T.);
#7641=EDGE_CURVE('',#6266,#6265,#3740,.T.);
#7642=EDGE_CURVE('',#6267,#6267,#5310,.T.);
#7643=EDGE_CURVE('',#6267,#6268,#3741,.T.);
#7644=EDGE_CURVE('',#6268,#6268,#5311,.T.);
#7645=EDGE_CURVE('',#6269,#6269,#5312,.T.);
#7646=EDGE_CURVE('',#6270,#6270,#5313,.T.);
#7647=EDGE_CURVE('',#6270,#6269,#3742,.T.);
#7648=EDGE_CURVE('',#6271,#6271,#5314,.T.);
#7649=EDGE_CURVE('',#6271,#6272,#3743,.T.);
#7650=EDGE_CURVE('',#6272,#6272,#5315,.T.);
#7651=EDGE_CURVE('',#6273,#6273,#5316,.T.);
#7652=EDGE_CURVE('',#6273,#6274,#3744,.T.);
#7653=EDGE_CURVE('',#6274,#6274,#5317,.T.);
#7654=EDGE_CURVE('',#6275,#6276,#3745,.T.);
#7655=EDGE_CURVE('',#6276,#6277,#3746,.T.);
#7656=EDGE_CURVE('',#6278,#6277,#3747,.T.);
#7657=EDGE_CURVE('',#6275,#6278,#3748,.T.);
#7658=EDGE_CURVE('',#6279,#6275,#3749,.T.);
#7659=EDGE_CURVE('',#6280,#6278,#3750,.T.);
#7660=EDGE_CURVE('',#6279,#6280,#3751,.T.);
#7661=EDGE_CURVE('',#6281,#6279,#3752,.T.);
#7662=EDGE_CURVE('',#6282,#6280,#3753,.T.);
#7663=EDGE_CURVE('',#6281,#6282,#3754,.T.);
#7664=EDGE_CURVE('',#6276,#6281,#3755,.T.);
#7665=EDGE_CURVE('',#6277,#6282,#3756,.T.);
#7666=EDGE_CURVE('',#6283,#6283,#5318,.T.);
#7667=EDGE_CURVE('',#6283,#6284,#3757,.T.);
#7668=EDGE_CURVE('',#6284,#6284,#5319,.T.);
#7669=EDGE_CURVE('',#6285,#6285,#5320,.T.);
#7670=EDGE_CURVE('',#6285,#6286,#3758,.T.);
#7671=EDGE_CURVE('',#6286,#6286,#5321,.T.);
#7672=EDGE_CURVE('',#6287,#6287,#5322,.T.);
#7673=EDGE_CURVE('',#6287,#6288,#3759,.T.);
#7674=EDGE_CURVE('',#6288,#6288,#5323,.T.);
#7675=EDGE_CURVE('',#6289,#6289,#5324,.T.);
#7676=EDGE_CURVE('',#6289,#6290,#3760,.T.);
#7677=EDGE_CURVE('',#6290,#6290,#5325,.T.);
#7678=EDGE_CURVE('',#6291,#6291,#5326,.T.);
#7679=EDGE_CURVE('',#6291,#6292,#3761,.T.);
#7680=EDGE_CURVE('',#6292,#6292,#5327,.T.);
#7681=EDGE_CURVE('',#6293,#6293,#5328,.T.);
#7682=EDGE_CURVE('',#6294,#6294,#5329,.T.);
#7683=EDGE_CURVE('',#6294,#6293,#3762,.T.);
#7684=EDGE_CURVE('',#6295,#6295,#5330,.T.);
#7685=EDGE_CURVE('',#6295,#6296,#3763,.T.);
#7686=EDGE_CURVE('',#6296,#6296,#5331,.T.);
#7687=EDGE_CURVE('',#6297,#6297,#5332,.T.);
#7688=EDGE_CURVE('',#6298,#6298,#5333,.T.);
#7689=EDGE_CURVE('',#6298,#6297,#3764,.T.);
#7690=EDGE_CURVE('',#6299,#6299,#5334,.T.);
#7691=EDGE_CURVE('',#6299,#6300,#3765,.T.);
#7692=EDGE_CURVE('',#6300,#6300,#5335,.T.);
#7693=EDGE_CURVE('',#6301,#6301,#5336,.T.);
#7694=EDGE_CURVE('',#6302,#6302,#5337,.T.);
#7695=EDGE_CURVE('',#6302,#6301,#3766,.T.);
#7696=EDGE_CURVE('',#6303,#6303,#5338,.T.);
#7697=EDGE_CURVE('',#6303,#6304,#3767,.T.);
#7698=EDGE_CURVE('',#6304,#6304,#5339,.T.);
#7699=EDGE_CURVE('',#6305,#6305,#5340,.T.);
#7700=EDGE_CURVE('',#6306,#6306,#5341,.T.);
#7701=EDGE_CURVE('',#6306,#6305,#3768,.T.);
#7702=EDGE_CURVE('',#6307,#6307,#5342,.T.);
#7703=EDGE_CURVE('',#6307,#6308,#3769,.T.);
#7704=EDGE_CURVE('',#6308,#6308,#5343,.T.);
#7705=EDGE_CURVE('',#6309,#6309,#5344,.T.);
#7706=EDGE_CURVE('',#6309,#6310,#3770,.T.);
#7707=EDGE_CURVE('',#6310,#6310,#5345,.T.);
#7708=EDGE_CURVE('',#6311,#6312,#3771,.T.);
#7709=EDGE_CURVE('',#6312,#6313,#3772,.T.);
#7710=EDGE_CURVE('',#6314,#6313,#3773,.T.);
#7711=EDGE_CURVE('',#6311,#6314,#3774,.T.);
#7712=EDGE_CURVE('',#6315,#6311,#3775,.T.);
#7713=EDGE_CURVE('',#6316,#6314,#3776,.T.);
#7714=EDGE_CURVE('',#6315,#6316,#3777,.T.);
#7715=EDGE_CURVE('',#6317,#6315,#3778,.T.);
#7716=EDGE_CURVE('',#6318,#6316,#3779,.T.);
#7717=EDGE_CURVE('',#6317,#6318,#3780,.T.);
#7718=EDGE_CURVE('',#6312,#6317,#3781,.T.);
#7719=EDGE_CURVE('',#6313,#6318,#3782,.T.);
#7720=EDGE_CURVE('',#6319,#6319,#5346,.T.);
#7721=EDGE_CURVE('',#6319,#6320,#3783,.T.);
#7722=EDGE_CURVE('',#6320,#6320,#5347,.T.);
#7723=EDGE_CURVE('',#6321,#6321,#5348,.T.);
#7724=EDGE_CURVE('',#6321,#6322,#3784,.T.);
#7725=EDGE_CURVE('',#6322,#6322,#5349,.T.);
#7726=EDGE_CURVE('',#6323,#6323,#5350,.T.);
#7727=EDGE_CURVE('',#6323,#6324,#3785,.T.);
#7728=EDGE_CURVE('',#6324,#6324,#5351,.T.);
#7729=EDGE_CURVE('',#6325,#6325,#5352,.T.);
#7730=EDGE_CURVE('',#6325,#6326,#3786,.T.);
#7731=EDGE_CURVE('',#6326,#6326,#5353,.T.);
#7732=EDGE_CURVE('',#6327,#6327,#5354,.T.);
#7733=EDGE_CURVE('',#6327,#6328,#3787,.T.);
#7734=EDGE_CURVE('',#6328,#6328,#5355,.T.);
#7735=EDGE_CURVE('',#6329,#6329,#5356,.T.);
#7736=EDGE_CURVE('',#6330,#6330,#5357,.T.);
#7737=EDGE_CURVE('',#6330,#6329,#3788,.T.);
#7738=EDGE_CURVE('',#6331,#6331,#5358,.T.);
#7739=EDGE_CURVE('',#6331,#6332,#3789,.T.);
#7740=EDGE_CURVE('',#6332,#6332,#5359,.T.);
#7741=EDGE_CURVE('',#6333,#6333,#5360,.T.);
#7742=EDGE_CURVE('',#6334,#6334,#5361,.T.);
#7743=EDGE_CURVE('',#6334,#6333,#3790,.T.);
#7744=EDGE_CURVE('',#6335,#6336,#3791,.T.);
#7745=EDGE_CURVE('',#6336,#6337,#3792,.T.);
#7746=EDGE_CURVE('',#6338,#6337,#3793,.T.);
#7747=EDGE_CURVE('',#6335,#6338,#3794,.T.);
#7748=EDGE_CURVE('',#6339,#6335,#3795,.T.);
#7749=EDGE_CURVE('',#6340,#6338,#3796,.T.);
#7750=EDGE_CURVE('',#6339,#6340,#3797,.T.);
#7751=EDGE_CURVE('',#6341,#6339,#3798,.T.);
#7752=EDGE_CURVE('',#6342,#6340,#3799,.T.);
#7753=EDGE_CURVE('',#6341,#6342,#3800,.T.);
#7754=EDGE_CURVE('',#6336,#6341,#3801,.T.);
#7755=EDGE_CURVE('',#6337,#6342,#3802,.T.);
#7756=EDGE_CURVE('',#6343,#6344,#3803,.T.);
#7757=EDGE_CURVE('',#6344,#6345,#3804,.T.);
#7758=EDGE_CURVE('',#6346,#6345,#3805,.T.);
#7759=EDGE_CURVE('',#6343,#6346,#3806,.T.);
#7760=EDGE_CURVE('',#6347,#6343,#3807,.T.);
#7761=EDGE_CURVE('',#6348,#6346,#3808,.T.);
#7762=EDGE_CURVE('',#6347,#6348,#3809,.T.);
#7763=EDGE_CURVE('',#6349,#6347,#3810,.T.);
#7764=EDGE_CURVE('',#6350,#6348,#3811,.T.);
#7765=EDGE_CURVE('',#6349,#6350,#3812,.T.);
#7766=EDGE_CURVE('',#6344,#6349,#3813,.T.);
#7767=EDGE_CURVE('',#6345,#6350,#3814,.T.);
#7768=EDGE_CURVE('',#6351,#6351,#5362,.T.);
#7769=EDGE_CURVE('',#6351,#6352,#3815,.T.);
#7770=EDGE_CURVE('',#6352,#6352,#5363,.T.);
#7771=EDGE_CURVE('',#6353,#6353,#5364,.T.);
#7772=EDGE_CURVE('',#6353,#6354,#3816,.T.);
#7773=EDGE_CURVE('',#6354,#6354,#5365,.T.);
#7774=EDGE_CURVE('',#6355,#6356,#3817,.T.);
#7775=EDGE_CURVE('',#6356,#6357,#3818,.T.);
#7776=EDGE_CURVE('',#6358,#6357,#3819,.T.);
#7777=EDGE_CURVE('',#6355,#6358,#3820,.T.);
#7778=EDGE_CURVE('',#6359,#6355,#3821,.T.);
#7779=EDGE_CURVE('',#6360,#6358,#3822,.T.);
#7780=EDGE_CURVE('',#6359,#6360,#3823,.T.);
#7781=EDGE_CURVE('',#6361,#6359,#3824,.T.);
#7782=EDGE_CURVE('',#6362,#6360,#3825,.T.);
#7783=EDGE_CURVE('',#6361,#6362,#3826,.T.);
#7784=EDGE_CURVE('',#6356,#6361,#3827,.T.);
#7785=EDGE_CURVE('',#6357,#6362,#3828,.T.);
#7786=EDGE_CURVE('',#6363,#6363,#5366,.T.);
#7787=EDGE_CURVE('',#6363,#6364,#3829,.T.);
#7788=EDGE_CURVE('',#6364,#6364,#5367,.T.);
#7789=EDGE_CURVE('',#6365,#6365,#5368,.T.);
#7790=EDGE_CURVE('',#6365,#6366,#3830,.T.);
#7791=EDGE_CURVE('',#6366,#6366,#5369,.T.);
#7792=EDGE_CURVE('',#6367,#6368,#3831,.T.);
#7793=EDGE_CURVE('',#6368,#6369,#3832,.T.);
#7794=EDGE_CURVE('',#6370,#6369,#3833,.T.);
#7795=EDGE_CURVE('',#6367,#6370,#3834,.T.);
#7796=EDGE_CURVE('',#6371,#6367,#3835,.T.);
#7797=EDGE_CURVE('',#6372,#6370,#3836,.T.);
#7798=EDGE_CURVE('',#6371,#6372,#3837,.T.);
#7799=EDGE_CURVE('',#6373,#6371,#3838,.T.);
#7800=EDGE_CURVE('',#6374,#6372,#3839,.T.);
#7801=EDGE_CURVE('',#6373,#6374,#3840,.T.);
#7802=EDGE_CURVE('',#6368,#6373,#3841,.T.);
#7803=EDGE_CURVE('',#6369,#6374,#3842,.T.);
#7804=EDGE_CURVE('',#6375,#6375,#5370,.T.);
#7805=EDGE_CURVE('',#6375,#6376,#3843,.T.);
#7806=EDGE_CURVE('',#6376,#6376,#5371,.T.);
#7807=EDGE_CURVE('',#6377,#6377,#5372,.T.);
#7808=EDGE_CURVE('',#6377,#6378,#3844,.T.);
#7809=EDGE_CURVE('',#6378,#6378,#5373,.T.);
#7810=EDGE_CURVE('',#6379,#6379,#5374,.T.);
#7811=EDGE_CURVE('',#6379,#6380,#3845,.T.);
#7812=EDGE_CURVE('',#6380,#6380,#5375,.T.);
#7813=EDGE_CURVE('',#6381,#6381,#5376,.T.);
#7814=EDGE_CURVE('',#6381,#6382,#3846,.T.);
#7815=EDGE_CURVE('',#6382,#6382,#5377,.T.);
#7816=EDGE_CURVE('',#6383,#6384,#3847,.T.);
#7817=EDGE_CURVE('',#6383,#6385,#3848,.T.);
#7818=EDGE_CURVE('',#6386,#6385,#3849,.T.);
#7819=EDGE_CURVE('',#6384,#6386,#3850,.T.);
#7820=EDGE_CURVE('',#6384,#6387,#3851,.T.);
#7821=EDGE_CURVE('',#6388,#6386,#3852,.T.);
#7822=EDGE_CURVE('',#6387,#6388,#3853,.T.);
#7823=EDGE_CURVE('',#6387,#6389,#3854,.T.);
#7824=EDGE_CURVE('',#6390,#6388,#3855,.T.);
#7825=EDGE_CURVE('',#6389,#6390,#3856,.T.);
#7826=EDGE_CURVE('',#6389,#6383,#3857,.T.);
#7827=EDGE_CURVE('',#6385,#6390,#3858,.T.);
#7828=EDGE_CURVE('',#6391,#6392,#5378,.T.);
#7829=EDGE_CURVE('',#6392,#6391,#5379,.T.);
#7830=EDGE_CURVE('',#6392,#6393,#5380,.T.);
#7831=EDGE_CURVE('',#6394,#6393,#5381,.T.);
#7832=EDGE_CURVE('',#6393,#6394,#5382,.T.);
#7833=EDGE_CURVE('',#6394,#6395,#3859,.T.);
#7834=EDGE_CURVE('',#6395,#6395,#5383,.T.);
#7835=EDGE_CURVE('',#6396,#6396,#5384,.T.);
#7836=EDGE_CURVE('',#6396,#6397,#3860,.T.);
#7837=EDGE_CURVE('',#6397,#6397,#5385,.T.);
#7838=EDGE_CURVE('',#6397,#6398,#3861,.T.);
#7839=EDGE_CURVE('',#6398,#6398,#5386,.T.);
#7840=EDGE_CURVE('',#6399,#6399,#5387,.T.);
#7841=EDGE_CURVE('',#6399,#6391,#3862,.T.);
#7842=EDGE_CURVE('',#6400,#6400,#5388,.T.);
#7843=EDGE_CURVE('',#6400,#6396,#3863,.T.);
#7844=EDGE_CURVE('',#6401,#6402,#5389,.T.);
#7845=EDGE_CURVE('',#6402,#6401,#5390,.T.);
#7846=EDGE_CURVE('',#6402,#6403,#5391,.T.);
#7847=EDGE_CURVE('',#6404,#6403,#5392,.T.);
#7848=EDGE_CURVE('',#6403,#6404,#5393,.T.);
#7849=EDGE_CURVE('',#6405,#6405,#5394,.T.);
#7850=EDGE_CURVE('',#6405,#6404,#3864,.T.);
#7851=EDGE_CURVE('',#6406,#6406,#5395,.T.);
#7852=EDGE_CURVE('',#6407,#6407,#5396,.T.);
#7853=EDGE_CURVE('',#6408,#6408,#5397,.T.);
#7854=EDGE_CURVE('',#6408,#6406,#3865,.T.);
#7855=EDGE_CURVE('',#6409,#6409,#5398,.T.);
#7856=EDGE_CURVE('',#6409,#6408,#3866,.T.);
#7857=EDGE_CURVE('',#6410,#6410,#5399,.T.);
#7858=EDGE_CURVE('',#6410,#6409,#3867,.T.);
#7859=EDGE_CURVE('',#6401,#6407,#3868,.T.);
#7860=EDGE_CURVE('',#6411,#6412,#5400,.T.);
#7861=EDGE_CURVE('',#6413,#6414,#5401,.T.);
#7862=EDGE_CURVE('',#6415,#6416,#5402,.T.);
#7863=EDGE_CURVE('',#6417,#6418,#5403,.T.);
#7864=EDGE_CURVE('',#6419,#6420,#5404,.T.);
#7865=EDGE_CURVE('',#6421,#6422,#5405,.T.);
#7866=EDGE_CURVE('',#6423,#6424,#5406,.T.);
#7867=EDGE_CURVE('',#6425,#6426,#5407,.T.);
#7868=EDGE_CURVE('',#6427,#6428,#521,.T.);
#7869=EDGE_CURVE('',#6429,#6427,#5408,.T.);
#7870=EDGE_CURVE('',#6430,#6429,#522,.T.);
#7871=EDGE_CURVE('',#6428,#6430,#5409,.T.);
#7872=EDGE_CURVE('',#6431,#6429,#5410,.T.);
#7873=EDGE_CURVE('',#6431,#6432,#523,.T.);
#7874=EDGE_CURVE('',#6433,#6432,#5411,.T.);
#7875=EDGE_CURVE('',#6433,#6434,#524,.T.);
#7876=EDGE_CURVE('',#6435,#6434,#5412,.T.);
#7877=EDGE_CURVE('',#6435,#6436,#525,.T.);
#7878=EDGE_CURVE('',#6436,#6437,#3869,.T.);
#7879=EDGE_CURVE('',#6437,#6437,#5413,.T.);
#7880=EDGE_CURVE('',#6436,#6438,#526,.T.);
#7881=EDGE_CURVE('',#6439,#6438,#5414,.T.);
#7882=EDGE_CURVE('',#6439,#6440,#527,.T.);
#7883=EDGE_CURVE('',#6441,#6440,#5415,.T.);
#7884=EDGE_CURVE('',#6441,#6442,#528,.T.);
#7885=EDGE_CURVE('',#6443,#6442,#5416,.T.);
#7886=EDGE_CURVE('',#6443,#6444,#529,.T.);
#7887=EDGE_CURVE('',#6445,#6444,#5417,.T.);
#7888=EDGE_CURVE('',#6445,#6446,#530,.T.);
#7889=EDGE_CURVE('',#6430,#6446,#5418,.T.);
#7890=EDGE_CURVE('',#6427,#6447,#5419,.T.);
#7891=EDGE_CURVE('',#6447,#6431,#5420,.T.);
#7892=EDGE_CURVE('',#6448,#6447,#531,.T.);
#7893=EDGE_CURVE('',#6432,#6448,#5421,.T.);
#7894=EDGE_CURVE('',#6448,#6449,#5422,.T.);
#7895=EDGE_CURVE('',#6449,#6433,#5423,.T.);
#7896=EDGE_CURVE('',#6450,#6449,#532,.T.);
#7897=EDGE_CURVE('',#6434,#6450,#5424,.T.);
#7898=EDGE_CURVE('',#6450,#6451,#5425,.T.);
#7899=EDGE_CURVE('',#6451,#6435,#5426,.T.);
#7900=EDGE_CURVE('',#6452,#6453,#533,.T.);
#7901=EDGE_CURVE('',#6438,#6452,#5427,.T.);
#7902=EDGE_CURVE('',#6453,#6451,#534,.T.);
#7903=EDGE_CURVE('',#6452,#6454,#5428,.T.);
#7904=EDGE_CURVE('',#6454,#6439,#5429,.T.);
#7905=EDGE_CURVE('',#6455,#6454,#535,.T.);
#7906=EDGE_CURVE('',#6440,#6455,#5430,.T.);
#7907=EDGE_CURVE('',#6455,#6456,#5431,.T.);
#7908=EDGE_CURVE('',#6456,#6441,#5432,.T.);
#7909=EDGE_CURVE('',#6457,#6456,#536,.T.);
#7910=EDGE_CURVE('',#6442,#6457,#5433,.T.);
#7911=EDGE_CURVE('',#6457,#6458,#5434,.T.);
#7912=EDGE_CURVE('',#6458,#6443,#5435,.T.);
#7913=EDGE_CURVE('',#6459,#6458,#537,.T.);
#7914=EDGE_CURVE('',#6444,#6459,#5436,.T.);
#7915=EDGE_CURVE('',#6460,#6460,#5437,.T.);
#7916=EDGE_CURVE('',#6460,#6453,#3870,.T.);
#7917=EDGE_CURVE('',#6461,#6428,#5438,.T.);
#7918=EDGE_CURVE('',#6461,#6462,#538,.T.);
#7919=EDGE_CURVE('',#6459,#6462,#5439,.T.);
#7920=EDGE_CURVE('',#6446,#6461,#5440,.T.);
#7921=EDGE_CURVE('',#6462,#6445,#5441,.T.);
#7922=EDGE_CURVE('',#6463,#6463,#5442,.T.);
#7923=EDGE_CURVE('',#6464,#6464,#5443,.T.);
#7924=EDGE_CURVE('',#6465,#6465,#5444,.T.);
#7925=EDGE_CURVE('',#6465,#6463,#3871,.T.);
#7926=EDGE_CURVE('',#6466,#6466,#5445,.T.);
#7927=EDGE_CURVE('',#6466,#6464,#3872,.T.);
#7928=EDGE_CURVE('',#6467,#6467,#5446,.T.);
#7929=EDGE_CURVE('',#6468,#6468,#5447,.T.);
#7930=EDGE_CURVE('',#6469,#6469,#5448,.T.);
#7931=EDGE_CURVE('',#6469,#6467,#3873,.T.);
#7932=EDGE_CURVE('',#6470,#6470,#5449,.T.);
#7933=EDGE_CURVE('',#6470,#6468,#3874,.T.);
#7934=EDGE_CURVE('',#6471,#6472,#3875,.T.);
#7935=EDGE_CURVE('',#6472,#6473,#3876,.T.);
#7936=EDGE_CURVE('',#6473,#6474,#3877,.T.);
#7937=EDGE_CURVE('',#6471,#6474,#3878,.T.);
#7938=EDGE_CURVE('',#6472,#6475,#3879,.T.);
#7939=EDGE_CURVE('',#6475,#6476,#3880,.T.);
#7940=EDGE_CURVE('',#6476,#6473,#3881,.T.);
#7941=EDGE_CURVE('',#6475,#6477,#3882,.T.);
#7942=EDGE_CURVE('',#6477,#6478,#3883,.T.);
#7943=EDGE_CURVE('',#6478,#6476,#3884,.T.);
#7944=EDGE_CURVE('',#6477,#6479,#3885,.T.);
#7945=EDGE_CURVE('',#6479,#6480,#3886,.T.);
#7946=EDGE_CURVE('',#6480,#6478,#3887,.T.);
#7947=EDGE_CURVE('',#6479,#6481,#3888,.T.);
#7948=EDGE_CURVE('',#6481,#6482,#3889,.T.);
#7949=EDGE_CURVE('',#6482,#6480,#3890,.T.);
#7950=EDGE_CURVE('',#6481,#6471,#3891,.T.);
#7951=EDGE_CURVE('',#6474,#6482,#3892,.T.);
#7952=EDGE_CURVE('',#6483,#6483,#5450,.T.);
#7953=EDGE_CURVE('',#6484,#6484,#5451,.T.);
#7954=EDGE_CURVE('',#6483,#6485,#3893,.T.);
#7955=EDGE_CURVE('',#6485,#6485,#5452,.T.);
#7956=EDGE_CURVE('',#6486,#6486,#5453,.T.);
#7957=EDGE_CURVE('',#6487,#6487,#5454,.T.);
#7958=EDGE_CURVE('',#6487,#6486,#3894,.T.);
#7959=EDGE_CURVE('',#6488,#6488,#5455,.T.);
#7960=EDGE_CURVE('',#6488,#6487,#3895,.T.);
#7961=EDGE_CURVE('',#6489,#6489,#5456,.T.);
#7962=EDGE_CURVE('',#6489,#6488,#3896,.T.);
#7963=EDGE_CURVE('',#6490,#6490,#5457,.T.);
#7964=EDGE_CURVE('',#6491,#6491,#5458,.F.);
#7965=EDGE_CURVE('',#6491,#6490,#3897,.T.);
#7966=EDGE_CURVE('',#6492,#6492,#5459,.F.);
#7967=EDGE_CURVE('',#6492,#6491,#3898,.T.);
#7968=EDGE_CURVE('',#6484,#6492,#3899,.T.);
#7969=EDGE_CURVE('',#6493,#6494,#5460,.T.);
#7970=EDGE_CURVE('',#6494,#6493,#5461,.T.);
#7971=EDGE_CURVE('',#6494,#6495,#5462,.T.);
#7972=EDGE_CURVE('',#6496,#6495,#5463,.T.);
#7973=EDGE_CURVE('',#6495,#6496,#5464,.T.);
#7974=EDGE_CURVE('',#6496,#6497,#3900,.T.);
#7975=EDGE_CURVE('',#6497,#6497,#5465,.T.);
#7976=EDGE_CURVE('',#6498,#6498,#5466,.T.);
#7977=EDGE_CURVE('',#6498,#6499,#3901,.T.);
#7978=EDGE_CURVE('',#6499,#6499,#5467,.T.);
#7979=EDGE_CURVE('',#6499,#6500,#3902,.T.);
#7980=EDGE_CURVE('',#6500,#6500,#5468,.T.);
#7981=EDGE_CURVE('',#6501,#6501,#5469,.T.);
#7982=EDGE_CURVE('',#6501,#6493,#3903,.T.);
#7983=EDGE_CURVE('',#6502,#6502,#5470,.T.);
#7984=EDGE_CURVE('',#6502,#6498,#3904,.T.);
#7985=EDGE_CURVE('',#6503,#6504,#5471,.T.);
#7986=EDGE_CURVE('',#6504,#6503,#5472,.T.);
#7987=EDGE_CURVE('',#6504,#6505,#5473,.T.);
#7988=EDGE_CURVE('',#6506,#6505,#5474,.T.);
#7989=EDGE_CURVE('',#6505,#6506,#5475,.T.);
#7990=EDGE_CURVE('',#6507,#6507,#5476,.T.);
#7991=EDGE_CURVE('',#6507,#6506,#3905,.T.);
#7992=EDGE_CURVE('',#6508,#6508,#5477,.T.);
#7993=EDGE_CURVE('',#6509,#6509,#5478,.T.);
#7994=EDGE_CURVE('',#6510,#6510,#5479,.T.);
#7995=EDGE_CURVE('',#6510,#6508,#3906,.T.);
#7996=EDGE_CURVE('',#6511,#6511,#5480,.T.);
#7997=EDGE_CURVE('',#6511,#6510,#3907,.T.);
#7998=EDGE_CURVE('',#6512,#6512,#5481,.T.);
#7999=EDGE_CURVE('',#6512,#6511,#3908,.T.);
#8000=EDGE_CURVE('',#6503,#6509,#3909,.T.);
#8001=EDGE_CURVE('',#6513,#6514,#5482,.T.);
#8002=EDGE_CURVE('',#6515,#6516,#5483,.T.);
#8003=EDGE_CURVE('',#6517,#6518,#5484,.T.);
#8004=EDGE_CURVE('',#6519,#6520,#5485,.T.);
#8005=EDGE_CURVE('',#6521,#6522,#5486,.T.);
#8006=EDGE_CURVE('',#6523,#6524,#5487,.T.);
#8007=EDGE_CURVE('',#6525,#6526,#5488,.T.);
#8008=EDGE_CURVE('',#6527,#6528,#539,.T.);
#8009=EDGE_CURVE('',#6529,#6527,#5489,.T.);
#8010=EDGE_CURVE('',#6530,#6529,#540,.T.);
#8011=EDGE_CURVE('',#6528,#6530,#5490,.T.);
#8012=EDGE_CURVE('',#6531,#6529,#5491,.T.);
#8013=EDGE_CURVE('',#6531,#6532,#541,.T.);
#8014=EDGE_CURVE('',#6533,#6532,#5492,.T.);
#8015=EDGE_CURVE('',#6533,#6534,#542,.T.);
#8016=EDGE_CURVE('',#6535,#6534,#5493,.T.);
#8017=EDGE_CURVE('',#6535,#6536,#3910,.T.);
#8018=EDGE_CURVE('',#6536,#6536,#5494,.T.);
#8019=EDGE_CURVE('',#6537,#6535,#5495,.T.);
#8020=EDGE_CURVE('',#6537,#6538,#543,.T.);
#8021=EDGE_CURVE('',#6539,#6538,#5496,.T.);
#8022=EDGE_CURVE('',#6539,#6540,#544,.T.);
#8023=EDGE_CURVE('',#6541,#6540,#5497,.T.);
#8024=EDGE_CURVE('',#6541,#6542,#545,.T.);
#8025=EDGE_CURVE('',#6543,#6542,#5498,.T.);
#8026=EDGE_CURVE('',#6543,#6544,#546,.T.);
#8027=EDGE_CURVE('',#6530,#6544,#5499,.T.);
#8028=EDGE_CURVE('',#6527,#6545,#5500,.T.);
#8029=EDGE_CURVE('',#6545,#6531,#5501,.T.);
#8030=EDGE_CURVE('',#6546,#6545,#547,.T.);
#8031=EDGE_CURVE('',#6532,#6546,#5502,.T.);
#8032=EDGE_CURVE('',#6546,#6547,#5503,.T.);
#8033=EDGE_CURVE('',#6547,#6533,#5504,.T.);
#8034=EDGE_CURVE('',#6548,#6547,#548,.T.);
#8035=EDGE_CURVE('',#6534,#6548,#5505,.T.);
#8036=EDGE_CURVE('',#6548,#6549,#5506,.T.);
#8037=EDGE_CURVE('',#6549,#6550,#5507,.T.);
#8038=EDGE_CURVE('',#6550,#6537,#5508,.T.);
#8039=EDGE_CURVE('',#6551,#6550,#549,.T.);
#8040=EDGE_CURVE('',#6538,#6551,#5509,.T.);
#8041=EDGE_CURVE('',#6551,#6552,#5510,.T.);
#8042=EDGE_CURVE('',#6552,#6539,#5511,.T.);
#8043=EDGE_CURVE('',#6553,#6552,#550,.T.);
#8044=EDGE_CURVE('',#6540,#6553,#5512,.T.);
#8045=EDGE_CURVE('',#6553,#6554,#5513,.T.);
#8046=EDGE_CURVE('',#6554,#6541,#5514,.T.);
#8047=EDGE_CURVE('',#6555,#6554,#551,.T.);
#8048=EDGE_CURVE('',#6542,#6555,#5515,.T.);
#8049=EDGE_CURVE('',#6556,#6556,#5516,.T.);
#8050=EDGE_CURVE('',#6556,#6549,#3911,.T.);
#8051=EDGE_CURVE('',#6557,#6528,#5517,.T.);
#8052=EDGE_CURVE('',#6557,#6558,#552,.T.);
#8053=EDGE_CURVE('',#6555,#6558,#5518,.T.);
#8054=EDGE_CURVE('',#6544,#6557,#5519,.T.);
#8055=EDGE_CURVE('',#6558,#6543,#5520,.T.);
#8056=EDGE_CURVE('',#6559,#6559,#5521,.T.);
#8057=EDGE_CURVE('',#6560,#6560,#5522,.T.);
#8058=EDGE_CURVE('',#6561,#6561,#5523,.T.);
#8059=EDGE_CURVE('',#6561,#6559,#3912,.T.);
#8060=EDGE_CURVE('',#6562,#6562,#5524,.T.);
#8061=EDGE_CURVE('',#6562,#6560,#3913,.T.);
#8062=EDGE_CURVE('',#6563,#6563,#5525,.T.);
#8063=EDGE_CURVE('',#6564,#6564,#5526,.T.);
#8064=EDGE_CURVE('',#6565,#6565,#5527,.T.);
#8065=EDGE_CURVE('',#6565,#6563,#3914,.T.);
#8066=EDGE_CURVE('',#6566,#6566,#5528,.T.);
#8067=EDGE_CURVE('',#6566,#6564,#3915,.T.);
#8068=EDGE_CURVE('',#6567,#6567,#5529,.T.);
#8069=EDGE_CURVE('',#6568,#6568,#5530,.T.);
#8070=EDGE_CURVE('',#6568,#6567,#3916,.T.);
#8071=EDGE_CURVE('',#6569,#6569,#5531,.T.);
#8072=EDGE_CURVE('',#6569,#6568,#3917,.T.);
#8073=EDGE_CURVE('',#6570,#6570,#5532,.T.);
#8074=EDGE_CURVE('',#6570,#6569,#3918,.T.);
#8075=EDGE_CURVE('',#6571,#6571,#5533,.T.);
#8076=EDGE_CURVE('',#6572,#6572,#5534,.F.);
#8077=EDGE_CURVE('',#6572,#6571,#3919,.T.);
#8078=EDGE_CURVE('',#6573,#6573,#5535,.F.);
#8079=EDGE_CURVE('',#6573,#6572,#3920,.T.);
#8080=EDGE_CURVE('',#6574,#6574,#5536,.T.);
#8081=EDGE_CURVE('',#6574,#6573,#3921,.T.);
#8082=EDGE_CURVE('',#6575,#6576,#3922,.T.);
#8083=EDGE_CURVE('',#6576,#6577,#3923,.T.);
#8084=EDGE_CURVE('',#6577,#6578,#3924,.T.);
#8085=EDGE_CURVE('',#6575,#6578,#3925,.T.);
#8086=EDGE_CURVE('',#6576,#6579,#3926,.T.);
#8087=EDGE_CURVE('',#6579,#6580,#3927,.T.);
#8088=EDGE_CURVE('',#6580,#6577,#3928,.T.);
#8089=EDGE_CURVE('',#6579,#6581,#3929,.T.);
#8090=EDGE_CURVE('',#6581,#6582,#3930,.T.);
#8091=EDGE_CURVE('',#6582,#6580,#3931,.T.);
#8092=EDGE_CURVE('',#6581,#6583,#3932,.T.);
#8093=EDGE_CURVE('',#6583,#6584,#3933,.T.);
#8094=EDGE_CURVE('',#6584,#6582,#3934,.T.);
#8095=EDGE_CURVE('',#6583,#6585,#3935,.T.);
#8096=EDGE_CURVE('',#6585,#6586,#3936,.T.);
#8097=EDGE_CURVE('',#6586,#6584,#3937,.T.);
#8098=EDGE_CURVE('',#6585,#6575,#3938,.T.);
#8099=EDGE_CURVE('',#6578,#6586,#3939,.T.);
#8100=EDGE_CURVE('',#6587,#6587,#5537,.T.);
#8101=EDGE_CURVE('',#6587,#6588,#3940,.T.);
#8102=EDGE_CURVE('',#6588,#6588,#5538,.T.);
#8103=EDGE_CURVE('',#6589,#6589,#5539,.T.);
#8104=EDGE_CURVE('',#6589,#6590,#3941,.T.);
#8105=EDGE_CURVE('',#6590,#6590,#5540,.T.);
#8106=EDGE_CURVE('',#6591,#6592,#5541,.T.);
#8107=EDGE_CURVE('',#6593,#6594,#3942,.T.);
#8108=EDGE_CURVE('',#6593,#6595,#3943,.T.);
#8109=EDGE_CURVE('',#6594,#6595,#5542,.T.);
#8110=EDGE_CURVE('',#6596,#6597,#3944,.T.);
#8111=EDGE_CURVE('',#6598,#6596,#5543,.T.);
#8112=EDGE_CURVE('',#6598,#6597,#3945,.T.);
#8113=EDGE_CURVE('',#6599,#6600,#3946,.T.);
#8114=EDGE_CURVE('',#6601,#6599,#5544,.T.);
#8115=EDGE_CURVE('',#6601,#6600,#3947,.T.);
#8116=EDGE_CURVE('',#6600,#6593,#3948,.T.);
#8117=EDGE_CURVE('',#6595,#6601,#3949,.T.);
#8118=EDGE_CURVE('',#6602,#6603,#3950,.T.);
#8119=EDGE_CURVE('',#6602,#6604,#3951,.T.);
#8120=EDGE_CURVE('',#6603,#6604,#5545,.T.);
#8121=EDGE_CURVE('',#6597,#6602,#3952,.T.);
#8122=EDGE_CURVE('',#6604,#6598,#3953,.T.);
#8123=EDGE_CURVE('',#6605,#6606,#3954,.T.);
#8124=EDGE_CURVE('',#6606,#6607,#3955,.T.);
#8125=EDGE_CURVE('',#6607,#6608,#3956,.T.);
#8126=EDGE_CURVE('',#6608,#6605,#3957,.T.);
#8127=EDGE_CURVE('',#6609,#6609,#5546,.T.);
#8128=EDGE_CURVE('',#6610,#6610,#5547,.T.);
#8129=EDGE_CURVE('',#6603,#6611,#3958,.T.);
#8130=EDGE_CURVE('',#6611,#6612,#3959,.T.);
#8131=EDGE_CURVE('',#6612,#6599,#3960,.T.);
#8132=EDGE_CURVE('',#6594,#6613,#3961,.T.);
#8133=EDGE_CURVE('',#6613,#6614,#3962,.T.);
#8134=EDGE_CURVE('',#6614,#6596,#3963,.T.);
#8135=EDGE_CURVE('',#6613,#6614,#5548,.T.);
#8136=EDGE_CURVE('',#6611,#6612,#5549,.T.);
#8137=EDGE_CURVE('',#6615,#6616,#3964,.T.);
#8138=EDGE_CURVE('',#6615,#6617,#3965,.T.);
#8139=EDGE_CURVE('',#6617,#6618,#3966,.T.);
#8140=EDGE_CURVE('',#6616,#6618,#3967,.T.);
#8141=EDGE_CURVE('',#6619,#6615,#3968,.T.);
#8142=EDGE_CURVE('',#6619,#6620,#3969,.T.);
#8143=EDGE_CURVE('',#6620,#6617,#3970,.T.);
#8144=EDGE_CURVE('',#6621,#6619,#3971,.T.);
#8145=EDGE_CURVE('',#6621,#6622,#3972,.T.);
#8146=EDGE_CURVE('',#6622,#6620,#3973,.T.);
#8147=EDGE_CURVE('',#6616,#6621,#3974,.T.);
#8148=EDGE_CURVE('',#6618,#6622,#3975,.T.);
#8149=EDGE_CURVE('',#6623,#6623,#5550,.T.);
#8150=EDGE_CURVE('',#6623,#6610,#3976,.T.);
#8151=EDGE_CURVE('',#6624,#6624,#5551,.T.);
#8152=EDGE_CURVE('',#6624,#6609,#3977,.T.);
#8153=EDGE_CURVE('',#6625,#6626,#3978,.T.);
#8154=EDGE_CURVE('',#6626,#6605,#3979,.T.);
#8155=EDGE_CURVE('',#6625,#6608,#3980,.T.);
#8156=EDGE_CURVE('',#6627,#6625,#3981,.T.);
#8157=EDGE_CURVE('',#6627,#6607,#3982,.T.);
#8158=EDGE_CURVE('',#6628,#6627,#3983,.T.);
#8159=EDGE_CURVE('',#6628,#6606,#3984,.T.);
#8160=EDGE_CURVE('',#6626,#6628,#3985,.T.);
#8161=EDGE_CURVE('',#6629,#6629,#5552,.T.);
#8162=EDGE_CURVE('',#6629,#6630,#3986,.T.);
#8163=EDGE_CURVE('',#6630,#6630,#5553,.T.);
#8164=EDGE_CURVE('',#6631,#6631,#5554,.T.);
#8165=EDGE_CURVE('',#6632,#6633,#5555,.T.);
#8166=EDGE_CURVE('',#6634,#6634,#5556,.T.);
#8167=EDGE_CURVE('',#6635,#6636,#553,.T.);
#8168=EDGE_CURVE('',#6637,#6635,#554,.T.);
#8169=EDGE_CURVE('',#6636,#6637,#555,.T.);
#8170=EDGE_CURVE('',#6636,#6638,#3987,.T.);
#8171=EDGE_CURVE('',#6638,#6638,#556,.T.);
#8172=EDGE_CURVE('',#6639,#6639,#557,.T.);
#8173=EDGE_CURVE('',#6639,#6640,#3988,.T.);
#8174=EDGE_CURVE('',#6641,#6640,#558,.T.);
#8175=EDGE_CURVE('',#6642,#6641,#559,.T.);
#8176=EDGE_CURVE('',#6640,#6642,#560,.T.);
#8177=EDGE_CURVE('',#6643,#6643,#5557,.T.);
#8178=EDGE_CURVE('',#6643,#6644,#3989,.T.);
#8179=EDGE_CURVE('',#6644,#6644,#5558,.T.);
#8180=EDGE_CURVE('',#6645,#6646,#561,.T.);
#8181=EDGE_CURVE('',#6646,#6647,#562,.T.);
#8182=EDGE_CURVE('',#6647,#6645,#563,.T.);
#8183=EDGE_CURVE('',#6648,#6649,#564,.T.);
#8184=EDGE_CURVE('',#6649,#6650,#565,.T.);
#8185=EDGE_CURVE('',#6650,#6648,#566,.T.);
#8186=EDGE_CURVE('',#6651,#6652,#567,.T.);
#8187=EDGE_CURVE('',#6652,#6653,#568,.T.);
#8188=EDGE_CURVE('',#6653,#6651,#569,.T.);
#8189=EDGE_CURVE('',#6654,#6655,#570,.T.);
#8190=EDGE_CURVE('',#6655,#6656,#571,.T.);
#8191=EDGE_CURVE('',#6656,#6654,#572,.T.);
#8192=EDGE_CURVE('',#6647,#6657,#3990,.T.);
#8193=EDGE_CURVE('',#6657,#6657,#573,.T.);
#8194=EDGE_CURVE('',#6658,#6658,#574,.T.);
#8195=EDGE_CURVE('',#6658,#6650,#3991,.T.);
#8196=EDGE_CURVE('',#6653,#6659,#3992,.T.);
#8197=EDGE_CURVE('',#6659,#6659,#575,.T.);
#8198=EDGE_CURVE('',#6660,#6660,#576,.T.);
#8199=EDGE_CURVE('',#6660,#6656,#3993,.T.);
#8200=EDGE_CURVE('',#6661,#6661,#5559,.T.);
#8201=EDGE_CURVE('',#6662,#6662,#5560,.T.);
#8202=EDGE_CURVE('',#6663,#6663,#5561,.T.);
#8203=EDGE_CURVE('',#6663,#6662,#3994,.T.);
#8204=EDGE_CURVE('',#6664,#6664,#5562,.T.);
#8205=EDGE_CURVE('',#6664,#6661,#3995,.T.);
#8206=EDGE_CURVE('',#6665,#6665,#5563,.T.);
#8207=EDGE_CURVE('',#6665,#6666,#3996,.T.);
#8208=EDGE_CURVE('',#6666,#6666,#5564,.T.);
#8209=EDGE_CURVE('',#6667,#6667,#5565,.T.);
#8210=EDGE_CURVE('',#6667,#6668,#3997,.T.);
#8211=EDGE_CURVE('',#6668,#6668,#5566,.T.);
#8212=EDGE_CURVE('',#6669,#6670,#3998,.T.);
#8213=EDGE_CURVE('',#6670,#6671,#3999,.T.);
#8214=EDGE_CURVE('',#6671,#6672,#4000,.T.);
#8215=EDGE_CURVE('',#6669,#6672,#4001,.T.);
#8216=EDGE_CURVE('',#6670,#6673,#4002,.T.);
#8217=EDGE_CURVE('',#6673,#6674,#4003,.T.);
#8218=EDGE_CURVE('',#6674,#6671,#4004,.T.);
#8219=EDGE_CURVE('',#6673,#6675,#4005,.T.);
#8220=EDGE_CURVE('',#6675,#6676,#4006,.T.);
#8221=EDGE_CURVE('',#6676,#6674,#4007,.T.);
#8222=EDGE_CURVE('',#6675,#6677,#4008,.T.);
#8223=EDGE_CURVE('',#6677,#6678,#4009,.T.);
#8224=EDGE_CURVE('',#6678,#6676,#4010,.T.);
#8225=EDGE_CURVE('',#6677,#6679,#4011,.T.);
#8226=EDGE_CURVE('',#6679,#6680,#4012,.T.);
#8227=EDGE_CURVE('',#6680,#6678,#4013,.T.);
#8228=EDGE_CURVE('',#6679,#6669,#4014,.T.);
#8229=EDGE_CURVE('',#6672,#6680,#4015,.T.);
#8230=EDGE_CURVE('',#6681,#6681,#5567,.T.);
#8231=EDGE_CURVE('',#6682,#6682,#5568,.T.);
#8232=EDGE_CURVE('',#6683,#6683,#5569,.T.);
#8233=EDGE_CURVE('',#6683,#6682,#4016,.T.);
#8234=EDGE_CURVE('',#6684,#6684,#5570,.T.);
#8235=EDGE_CURVE('',#6684,#6683,#4017,.T.);
#8236=EDGE_CURVE('',#6685,#6685,#5571,.T.);
#8237=EDGE_CURVE('',#6685,#6684,#4018,.T.);
#8238=EDGE_CURVE('',#6686,#6686,#5572,.T.);
#8239=EDGE_CURVE('',#6687,#6687,#5573,.F.);
#8240=EDGE_CURVE('',#6687,#6686,#4019,.T.);
#8241=EDGE_CURVE('',#6681,#6687,#4020,.T.);
#8242=EDGE_CURVE('',#6688,#6689,#4021,.T.);
#8243=EDGE_CURVE('',#6689,#6690,#4022,.T.);
#8244=EDGE_CURVE('',#6690,#6691,#4023,.T.);
#8245=EDGE_CURVE('',#6688,#6691,#4024,.T.);
#8246=EDGE_CURVE('',#6689,#6692,#4025,.T.);
#8247=EDGE_CURVE('',#6692,#6693,#4026,.T.);
#8248=EDGE_CURVE('',#6693,#6690,#4027,.T.);
#8249=EDGE_CURVE('',#6692,#6694,#4028,.T.);
#8250=EDGE_CURVE('',#6694,#6695,#4029,.T.);
#8251=EDGE_CURVE('',#6695,#6693,#4030,.T.);
#8252=EDGE_CURVE('',#6694,#6696,#4031,.T.);
#8253=EDGE_CURVE('',#6696,#6697,#4032,.T.);
#8254=EDGE_CURVE('',#6697,#6695,#4033,.T.);
#8255=EDGE_CURVE('',#6696,#6698,#4034,.T.);
#8256=EDGE_CURVE('',#6698,#6699,#4035,.T.);
#8257=EDGE_CURVE('',#6699,#6697,#4036,.T.);
#8258=EDGE_CURVE('',#6698,#6688,#4037,.T.);
#8259=EDGE_CURVE('',#6691,#6699,#4038,.T.);
#8260=EDGE_CURVE('',#6700,#6700,#5574,.T.);
#8261=EDGE_CURVE('',#6701,#6701,#5575,.T.);
#8262=EDGE_CURVE('',#6702,#6702,#5576,.T.);
#8263=EDGE_CURVE('',#6702,#6701,#4039,.T.);
#8264=EDGE_CURVE('',#6703,#6703,#5577,.T.);
#8265=EDGE_CURVE('',#6703,#6702,#4040,.T.);
#8266=EDGE_CURVE('',#6704,#6704,#5578,.T.);
#8267=EDGE_CURVE('',#6704,#6703,#4041,.T.);
#8268=EDGE_CURVE('',#6705,#6705,#5579,.T.);
#8269=EDGE_CURVE('',#6706,#6706,#5580,.F.);
#8270=EDGE_CURVE('',#6706,#6705,#4042,.T.);
#8271=EDGE_CURVE('',#6700,#6706,#4043,.T.);
#8272=EDGE_CURVE('',#6707,#6707,#5581,.T.);
#8273=EDGE_CURVE('',#6707,#6708,#4044,.T.);
#8274=EDGE_CURVE('',#6708,#6708,#5582,.T.);
#8275=EDGE_CURVE('',#6709,#6709,#5583,.T.);
#8276=EDGE_CURVE('',#6710,#6710,#5584,.T.);
#8277=EDGE_CURVE('',#6711,#6711,#5585,.T.);
#8278=EDGE_CURVE('',#6712,#6712,#5586,.T.);
#8279=EDGE_CURVE('',#6709,#6711,#4045,.T.);
#8280=EDGE_CURVE('',#6712,#6713,#4046,.T.);
#8281=EDGE_CURVE('',#6713,#6713,#5587,.T.);
#8282=EDGE_CURVE('',#6714,#6714,#5588,.T.);
#8283=EDGE_CURVE('',#6714,#6715,#4047,.T.);
#8284=EDGE_CURVE('',#6715,#6715,#5589,.T.);
#8285=EDGE_CURVE('',#6716,#6716,#5590,.T.);
#8286=EDGE_CURVE('',#6716,#6710,#4048,.T.);
#8287=EDGE_CURVE('',#6717,#6717,#5591,.T.);
#8288=EDGE_CURVE('',#6717,#6718,#4049,.T.);
#8289=EDGE_CURVE('',#6718,#6718,#5592,.T.);
#8290=EDGE_CURVE('',#6719,#6719,#5593,.T.);
#8291=EDGE_CURVE('',#6719,#6720,#4050,.T.);
#8292=EDGE_CURVE('',#6720,#6720,#5594,.T.);
#8293=EDGE_CURVE('',#6721,#6721,#5595,.T.);
#8294=EDGE_CURVE('',#6721,#6722,#4051,.T.);
#8295=EDGE_CURVE('',#6722,#6722,#5596,.T.);
#8296=EDGE_CURVE('',#6723,#6723,#5597,.T.);
#8297=EDGE_CURVE('',#6723,#6724,#4052,.T.);
#8298=EDGE_CURVE('',#6724,#6724,#5598,.T.);
#8299=EDGE_CURVE('',#6725,#6725,#5599,.T.);
#8300=EDGE_CURVE('',#6725,#6726,#4053,.T.);
#8301=EDGE_CURVE('',#6726,#6726,#5600,.T.);
#8302=EDGE_CURVE('',#6727,#6727,#5601,.T.);
#8303=EDGE_CURVE('',#6727,#6728,#4054,.T.);
#8304=EDGE_CURVE('',#6728,#6728,#5602,.T.);
#8305=EDGE_CURVE('',#6729,#6729,#5603,.T.);
#8306=EDGE_CURVE('',#6729,#6730,#4055,.T.);
#8307=EDGE_CURVE('',#6730,#6730,#5604,.T.);
#8308=EDGE_CURVE('',#6731,#6731,#5605,.T.);
#8309=EDGE_CURVE('',#6731,#6732,#4056,.T.);
#8310=EDGE_CURVE('',#6732,#6732,#5606,.T.);
#8311=EDGE_CURVE('',#6733,#6733,#5607,.T.);
#8312=EDGE_CURVE('',#6733,#6734,#4057,.T.);
#8313=EDGE_CURVE('',#6734,#6734,#5608,.T.);
#8314=EDGE_CURVE('',#6735,#6735,#5609,.T.);
#8315=EDGE_CURVE('',#6735,#6736,#4058,.T.);
#8316=EDGE_CURVE('',#6736,#6736,#5610,.T.);
#8317=EDGE_CURVE('',#6737,#6738,#4059,.T.);
#8318=EDGE_CURVE('',#6737,#6738,#5611,.T.);
#8319=EDGE_CURVE('',#6739,#6737,#577,.T.);
#8320=EDGE_CURVE('',#6740,#6739,#5612,.T.);
#8321=EDGE_CURVE('',#6740,#6741,#4060,.T.);
#8322=EDGE_CURVE('',#6742,#6741,#578,.T.);
#8323=EDGE_CURVE('',#6741,#6742,#579,.T.);
#8324=EDGE_CURVE('',#6743,#6740,#5613,.T.);
#8325=EDGE_CURVE('',#6738,#6743,#580,.T.);
#8326=EDGE_CURVE('',#6743,#6739,#4061,.T.);
#8327=EDGE_CURVE('',#6744,#6745,#4062,.T.);
#8328=EDGE_CURVE('',#6744,#6745,#5614,.T.);
#8329=EDGE_CURVE('',#6746,#6744,#581,.T.);
#8330=EDGE_CURVE('',#6747,#6746,#5615,.T.);
#8331=EDGE_CURVE('',#6747,#6748,#4063,.T.);
#8332=EDGE_CURVE('',#6749,#6748,#582,.T.);
#8333=EDGE_CURVE('',#6748,#6749,#583,.T.);
#8334=EDGE_CURVE('',#6750,#6747,#5616,.T.);
#8335=EDGE_CURVE('',#6745,#6750,#584,.T.);
#8336=EDGE_CURVE('',#6750,#6746,#4064,.T.);
#8337=EDGE_CURVE('',#6751,#6751,#5617,.T.);
#8338=EDGE_CURVE('',#6751,#6752,#4065,.T.);
#8339=EDGE_CURVE('',#6752,#6752,#5618,.T.);
#8340=EDGE_CURVE('',#6753,#6753,#5619,.T.);
#8341=EDGE_CURVE('',#6753,#6754,#4066,.T.);
#8342=EDGE_CURVE('',#6754,#6754,#5620,.T.);
#8343=EDGE_CURVE('',#6755,#6756,#585,.T.);
#8344=EDGE_CURVE('',#6757,#6755,#586,.T.);
#8345=EDGE_CURVE('',#6756,#6757,#587,.T.);
#8346=EDGE_CURVE('',#6756,#6758,#4067,.T.);
#8347=EDGE_CURVE('',#6759,#6758,#588,.T.);
#8348=EDGE_CURVE('',#6760,#6759,#589,.T.);
#8349=EDGE_CURVE('',#6761,#6760,#590,.T.);
#8350=EDGE_CURVE('',#6758,#6761,#591,.T.);
#8351=EDGE_CURVE('',#6762,#6763,#592,.T.);
#8352=EDGE_CURVE('',#6763,#6762,#593,.T.);
#8353=EDGE_CURVE('',#6763,#6764,#4068,.T.);
#8354=EDGE_CURVE('',#6765,#6764,#594,.T.);
#8355=EDGE_CURVE('',#6766,#6765,#595,.T.);
#8356=EDGE_CURVE('',#6764,#6766,#596,.T.);
#8357=EDGE_CURVE('',#6767,#6767,#5621,.T.);
#8358=EDGE_CURVE('',#6767,#6757,#4069,.T.);
#8359=EDGE_CURVE('',#6755,#6768,#4070,.T.);
#8360=EDGE_CURVE('',#6768,#6768,#5622,.T.);
#8361=EDGE_CURVE('',#6769,#6770,#597,.T.);
#8362=EDGE_CURVE('',#6770,#6771,#598,.T.);
#8363=EDGE_CURVE('',#6771,#6769,#599,.T.);
#8364=EDGE_CURVE('',#6772,#6773,#600,.T.);
#8365=EDGE_CURVE('',#6773,#6774,#601,.T.);
#8366=EDGE_CURVE('',#6774,#6772,#602,.T.);
#8367=EDGE_CURVE('',#6771,#6775,#4071,.T.);
#8368=EDGE_CURVE('',#6776,#6775,#603,.T.);
#8369=EDGE_CURVE('',#6775,#6776,#604,.T.);
#8370=EDGE_CURVE('',#6777,#6778,#605,.T.);
#8371=EDGE_CURVE('',#6778,#6777,#606,.T.);
#8372=EDGE_CURVE('',#6778,#6774,#4072,.T.);
#8373=EDGE_CURVE('',#6779,#6779,#5623,.T.);
#8374=EDGE_CURVE('',#6779,#6759,#4073,.T.);
#8375=EDGE_CURVE('',#6761,#6780,#4074,.T.);
#8376=EDGE_CURVE('',#6780,#6780,#5624,.T.);
#8377=EDGE_CURVE('',#6781,#6781,#5625,.T.);
#8378=EDGE_CURVE('',#6782,#6783,#5626,.T.);
#8379=EDGE_CURVE('',#6784,#6783,#5627,.T.);
#8380=EDGE_CURVE('',#6784,#6785,#5628,.T.);
#8381=EDGE_CURVE('',#6786,#6785,#5629,.T.);
#8382=EDGE_CURVE('',#6786,#6787,#5630,.T.);
#8383=EDGE_CURVE('',#6788,#6787,#5631,.T.);
#8384=EDGE_CURVE('',#6788,#6789,#5632,.T.);
#8385=EDGE_CURVE('',#6790,#6789,#5633,.T.);
#8386=EDGE_CURVE('',#6790,#6791,#5634,.T.);
#8387=EDGE_CURVE('',#6792,#6791,#5635,.T.);
#8388=EDGE_CURVE('',#6792,#6793,#5636,.T.);
#8389=EDGE_CURVE('',#6794,#6793,#5637,.T.);
#8390=EDGE_CURVE('',#6794,#6795,#5638,.T.);
#8391=EDGE_CURVE('',#6796,#6795,#5639,.T.);
#8392=EDGE_CURVE('',#6796,#6797,#5640,.T.);
#8393=EDGE_CURVE('',#6798,#6797,#5641,.T.);
#8394=EDGE_CURVE('',#6798,#6799,#5642,.T.);
#8395=EDGE_CURVE('',#6800,#6799,#5643,.T.);
#8396=EDGE_CURVE('',#6800,#6801,#5644,.T.);
#8397=EDGE_CURVE('',#6802,#6801,#5645,.T.);
#8398=EDGE_CURVE('',#6802,#6803,#5646,.T.);
#8399=EDGE_CURVE('',#6804,#6803,#5647,.T.);
#8400=EDGE_CURVE('',#6804,#6805,#5648,.T.);
#8401=EDGE_CURVE('',#6806,#6805,#5649,.T.);
#8402=EDGE_CURVE('',#6806,#6807,#5650,.T.);
#8403=EDGE_CURVE('',#6808,#6807,#5651,.T.);
#8404=EDGE_CURVE('',#6808,#6809,#5652,.T.);
#8405=EDGE_CURVE('',#6810,#6809,#5653,.T.);
#8406=EDGE_CURVE('',#6810,#6811,#5654,.T.);
#8407=EDGE_CURVE('',#6812,#6811,#5655,.T.);
#8408=EDGE_CURVE('',#6812,#6813,#5656,.T.);
#8409=EDGE_CURVE('',#6814,#6813,#5657,.T.);
#8410=EDGE_CURVE('',#6814,#6815,#5658,.T.);
#8411=EDGE_CURVE('',#6816,#6815,#5659,.T.);
#8412=EDGE_CURVE('',#6816,#6817,#5660,.T.);
#8413=EDGE_CURVE('',#6818,#6817,#5661,.T.);
#8414=EDGE_CURVE('',#6818,#6819,#5662,.T.);
#8415=EDGE_CURVE('',#6820,#6819,#5663,.T.);
#8416=EDGE_CURVE('',#6820,#6821,#5664,.T.);
#8417=EDGE_CURVE('',#6782,#6821,#5665,.T.);
#8418=EDGE_CURVE('',#6822,#6822,#5666,.T.);
#8419=EDGE_CURVE('',#6822,#6781,#4075,.T.);
#8420=EDGE_CURVE('',#6823,#6823,#5667,.T.);
#8421=EDGE_CURVE('',#6824,#6825,#5668,.T.);
#8422=EDGE_CURVE('',#6825,#6826,#5669,.T.);
#8423=EDGE_CURVE('',#6826,#6827,#5670,.T.);
#8424=EDGE_CURVE('',#6827,#6828,#5671,.T.);
#8425=EDGE_CURVE('',#6828,#6829,#5672,.T.);
#8426=EDGE_CURVE('',#6829,#6830,#5673,.T.);
#8427=EDGE_CURVE('',#6830,#6831,#5674,.T.);
#8428=EDGE_CURVE('',#6831,#6832,#5675,.T.);
#8429=EDGE_CURVE('',#6832,#6833,#5676,.T.);
#8430=EDGE_CURVE('',#6833,#6834,#5677,.T.);
#8431=EDGE_CURVE('',#6834,#6835,#5678,.T.);
#8432=EDGE_CURVE('',#6835,#6836,#5679,.T.);
#8433=EDGE_CURVE('',#6836,#6837,#5680,.T.);
#8434=EDGE_CURVE('',#6837,#6838,#5681,.T.);
#8435=EDGE_CURVE('',#6838,#6839,#5682,.T.);
#8436=EDGE_CURVE('',#6839,#6840,#5683,.T.);
#8437=EDGE_CURVE('',#6840,#6841,#5684,.T.);
#8438=EDGE_CURVE('',#6841,#6842,#5685,.T.);
#8439=EDGE_CURVE('',#6842,#6843,#5686,.T.);
#8440=EDGE_CURVE('',#6843,#6844,#5687,.T.);
#8441=EDGE_CURVE('',#6844,#6845,#5688,.T.);
#8442=EDGE_CURVE('',#6845,#6846,#5689,.T.);
#8443=EDGE_CURVE('',#6846,#6847,#5690,.T.);
#8444=EDGE_CURVE('',#6847,#6848,#5691,.T.);
#8445=EDGE_CURVE('',#6848,#6849,#5692,.T.);
#8446=EDGE_CURVE('',#6849,#6850,#5693,.T.);
#8447=EDGE_CURVE('',#6850,#6851,#5694,.T.);
#8448=EDGE_CURVE('',#6851,#6852,#5695,.T.);
#8449=EDGE_CURVE('',#6852,#6853,#5696,.T.);
#8450=EDGE_CURVE('',#6853,#6854,#5697,.T.);
#8451=EDGE_CURVE('',#6854,#6855,#5698,.T.);
#8452=EDGE_CURVE('',#6855,#6856,#5699,.T.);
#8453=EDGE_CURVE('',#6856,#6857,#5700,.T.);
#8454=EDGE_CURVE('',#6857,#6858,#5701,.T.);
#8455=EDGE_CURVE('',#6858,#6859,#5702,.T.);
#8456=EDGE_CURVE('',#6859,#6860,#5703,.T.);
#8457=EDGE_CURVE('',#6860,#6861,#5704,.T.);
#8458=EDGE_CURVE('',#6861,#6862,#5705,.T.);
#8459=EDGE_CURVE('',#6862,#6863,#5706,.T.);
#8460=EDGE_CURVE('',#6863,#6824,#5707,.T.);
#8461=EDGE_CURVE('',#6864,#6864,#5708,.T.);
#8462=EDGE_CURVE('',#6864,#6823,#4076,.T.);
#8463=EDGE_CURVE('',#6825,#6782,#4077,.T.);
#8464=EDGE_CURVE('',#6783,#6824,#4078,.T.);
#8465=EDGE_CURVE('',#6863,#6784,#4079,.T.);
#8466=EDGE_CURVE('',#6785,#6862,#4080,.T.);
#8467=EDGE_CURVE('',#6861,#6786,#4081,.T.);
#8468=EDGE_CURVE('',#6787,#6860,#4082,.T.);
#8469=EDGE_CURVE('',#6859,#6788,#4083,.T.);
#8470=EDGE_CURVE('',#6789,#6858,#4084,.T.);
#8471=EDGE_CURVE('',#6857,#6790,#4085,.T.);
#8472=EDGE_CURVE('',#6791,#6856,#4086,.T.);
#8473=EDGE_CURVE('',#6855,#6792,#4087,.T.);
#8474=EDGE_CURVE('',#6793,#6854,#4088,.T.);
#8475=EDGE_CURVE('',#6853,#6794,#4089,.T.);
#8476=EDGE_CURVE('',#6795,#6852,#4090,.T.);
#8477=EDGE_CURVE('',#6851,#6796,#4091,.T.);
#8478=EDGE_CURVE('',#6797,#6850,#4092,.T.);
#8479=EDGE_CURVE('',#6849,#6798,#4093,.T.);
#8480=EDGE_CURVE('',#6799,#6848,#4094,.T.);
#8481=EDGE_CURVE('',#6847,#6800,#4095,.T.);
#8482=EDGE_CURVE('',#6801,#6846,#4096,.T.);
#8483=EDGE_CURVE('',#6845,#6802,#4097,.T.);
#8484=EDGE_CURVE('',#6803,#6844,#4098,.T.);
#8485=EDGE_CURVE('',#6843,#6804,#4099,.T.);
#8486=EDGE_CURVE('',#6805,#6842,#4100,.T.);
#8487=EDGE_CURVE('',#6841,#6806,#4101,.T.);
#8488=EDGE_CURVE('',#6807,#6840,#4102,.T.);
#8489=EDGE_CURVE('',#6839,#6808,#4103,.T.);
#8490=EDGE_CURVE('',#6809,#6838,#4104,.T.);
#8491=EDGE_CURVE('',#6837,#6810,#4105,.T.);
#8492=EDGE_CURVE('',#6811,#6836,#4106,.T.);
#8493=EDGE_CURVE('',#6835,#6812,#4107,.T.);
#8494=EDGE_CURVE('',#6813,#6834,#4108,.T.);
#8495=EDGE_CURVE('',#6833,#6814,#4109,.T.);
#8496=EDGE_CURVE('',#6815,#6832,#4110,.T.);
#8497=EDGE_CURVE('',#6831,#6816,#4111,.T.);
#8498=EDGE_CURVE('',#6817,#6830,#4112,.T.);
#8499=EDGE_CURVE('',#6829,#6818,#4113,.T.);
#8500=EDGE_CURVE('',#6819,#6828,#4114,.T.);
#8501=EDGE_CURVE('',#6821,#6826,#4115,.T.);
#8502=EDGE_CURVE('',#6827,#6820,#4116,.T.);
#8503=EDGE_CURVE('',#6865,#6865,#5709,.T.);
#8504=EDGE_CURVE('',#6866,#6866,#5710,.T.);
#8505=EDGE_CURVE('',#6867,#6867,#5711,.T.);
#8506=EDGE_CURVE('',#6867,#6865,#4117,.T.);
#8507=EDGE_CURVE('',#6868,#6868,#5712,.T.);
#8508=EDGE_CURVE('',#6868,#6869,#4118,.T.);
#8509=EDGE_CURVE('',#6869,#6869,#5713,.T.);
#8510=EDGE_CURVE('',#6870,#6870,#5714,.T.);
#8511=EDGE_CURVE('',#6871,#6871,#5715,.T.);
#8512=EDGE_CURVE('',#6866,#6870,#4119,.T.);
#8513=EDGE_CURVE('',#6871,#6872,#4120,.T.);
#8514=EDGE_CURVE('',#6872,#6872,#5716,.T.);
#8515=EDGE_CURVE('',#6873,#6873,#5717,.T.);
#8516=EDGE_CURVE('',#6873,#6874,#4121,.T.);
#8517=EDGE_CURVE('',#6874,#6874,#5718,.T.);
#8518=EDGE_CURVE('',#6875,#6875,#5719,.T.);
#8519=EDGE_CURVE('',#6875,#6876,#4122,.T.);
#8520=EDGE_CURVE('',#6876,#6876,#5720,.T.);
#8521=EDGE_CURVE('',#6877,#6877,#5721,.T.);
#8522=EDGE_CURVE('',#6877,#6878,#4123,.T.);
#8523=EDGE_CURVE('',#6878,#6878,#5722,.T.);
#8524=EDGE_CURVE('',#6879,#6879,#5723,.T.);
#8525=EDGE_CURVE('',#6879,#6880,#4124,.T.);
#8526=EDGE_CURVE('',#6880,#6880,#5724,.T.);
#8527=EDGE_CURVE('',#6881,#6881,#5725,.T.);
#8528=EDGE_CURVE('',#6881,#6882,#4125,.T.);
#8529=EDGE_CURVE('',#6882,#6882,#5726,.T.);
#8530=EDGE_CURVE('',#6883,#6883,#5727,.T.);
#8531=EDGE_CURVE('',#6883,#6884,#4126,.T.);
#8532=EDGE_CURVE('',#6884,#6884,#5728,.T.);
#8533=EDGE_CURVE('',#6885,#6885,#5729,.T.);
#8534=EDGE_CURVE('',#6885,#6886,#4127,.T.);
#8535=EDGE_CURVE('',#6886,#6886,#5730,.T.);
#8536=EDGE_CURVE('',#6887,#6887,#5731,.T.);
#8537=EDGE_CURVE('',#6887,#6888,#4128,.T.);
#8538=EDGE_CURVE('',#6888,#6888,#5732,.T.);
#8539=EDGE_CURVE('',#6889,#6890,#4129,.T.);
#8540=EDGE_CURVE('',#6889,#6890,#5733,.T.);
#8541=EDGE_CURVE('',#6891,#6889,#607,.T.);
#8542=EDGE_CURVE('',#6892,#6891,#5734,.T.);
#8543=EDGE_CURVE('',#6892,#6893,#4130,.T.);
#8544=EDGE_CURVE('',#6894,#6893,#608,.T.);
#8545=EDGE_CURVE('',#6893,#6894,#609,.T.);
#8546=EDGE_CURVE('',#6895,#6892,#5735,.T.);
#8547=EDGE_CURVE('',#6890,#6895,#610,.T.);
#8548=EDGE_CURVE('',#6895,#6891,#4131,.T.);
#8549=EDGE_CURVE('',#6896,#6896,#5736,.T.);
#8550=EDGE_CURVE('',#6896,#6897,#4132,.T.);
#8551=EDGE_CURVE('',#6897,#6897,#5737,.T.);
#8552=EDGE_CURVE('',#6898,#6898,#5738,.T.);
#8553=EDGE_CURVE('',#6898,#6899,#4133,.T.);
#8554=EDGE_CURVE('',#6899,#6899,#5739,.T.);
#8555=EDGE_CURVE('',#6900,#6901,#4134,.T.);
#8556=EDGE_CURVE('',#6900,#6901,#5740,.T.);
#8557=EDGE_CURVE('',#6902,#6900,#611,.T.);
#8558=EDGE_CURVE('',#6903,#6902,#5741,.T.);
#8559=EDGE_CURVE('',#6903,#6904,#4135,.T.);
#8560=EDGE_CURVE('',#6905,#6904,#612,.T.);
#8561=EDGE_CURVE('',#6904,#6905,#613,.T.);
#8562=EDGE_CURVE('',#6906,#6903,#5742,.T.);
#8563=EDGE_CURVE('',#6901,#6906,#614,.T.);
#8564=EDGE_CURVE('',#6906,#6902,#4136,.T.);
#8565=EDGE_CURVE('',#6907,#6907,#5743,.T.);
#8566=EDGE_CURVE('',#6907,#6908,#4137,.T.);
#8567=EDGE_CURVE('',#6908,#6908,#5744,.T.);
#8568=EDGE_CURVE('',#6909,#6909,#5745,.T.);
#8569=EDGE_CURVE('',#6909,#6910,#4138,.T.);
#8570=EDGE_CURVE('',#6910,#6910,#5746,.T.);
#8571=EDGE_CURVE('',#6911,#6911,#5747,.T.);
#8572=EDGE_CURVE('',#6911,#6912,#4139,.T.);
#8573=EDGE_CURVE('',#6912,#6912,#5748,.T.);
#8574=EDGE_CURVE('',#6913,#6913,#5749,.T.);
#8575=EDGE_CURVE('',#6913,#6914,#4140,.T.);
#8576=EDGE_CURVE('',#6914,#6914,#5750,.T.);
#8577=EDGE_CURVE('',#6915,#6915,#5751,.T.);
#8578=EDGE_CURVE('',#6915,#6916,#4141,.T.);
#8579=EDGE_CURVE('',#6916,#6916,#5752,.T.);
#8580=EDGE_CURVE('',#6917,#6917,#5753,.T.);
#8581=EDGE_CURVE('',#6917,#6918,#4142,.T.);
#8582=EDGE_CURVE('',#6918,#6918,#5754,.T.);
#8583=EDGE_CURVE('',#6919,#6919,#5755,.T.);
#8584=EDGE_CURVE('',#6919,#6920,#4143,.T.);
#8585=EDGE_CURVE('',#6920,#6920,#5756,.T.);
#8586=EDGE_CURVE('',#6921,#6921,#5757,.T.);
#8587=EDGE_CURVE('',#6921,#6922,#4144,.T.);
#8588=EDGE_CURVE('',#6922,#6922,#5758,.T.);
#8589=EDGE_CURVE('',#6923,#6924,#4145,.T.);
#8590=EDGE_CURVE('',#6923,#6924,#5759,.T.);
#8591=EDGE_CURVE('',#6925,#6923,#615,.T.);
#8592=EDGE_CURVE('',#6926,#6925,#5760,.T.);
#8593=EDGE_CURVE('',#6926,#6927,#4146,.T.);
#8594=EDGE_CURVE('',#6928,#6927,#616,.T.);
#8595=EDGE_CURVE('',#6927,#6928,#617,.T.);
#8596=EDGE_CURVE('',#6929,#6926,#5761,.T.);
#8597=EDGE_CURVE('',#6924,#6929,#618,.T.);
#8598=EDGE_CURVE('',#6929,#6925,#4147,.T.);
#8599=EDGE_CURVE('',#6930,#6930,#5762,.T.);
#8600=EDGE_CURVE('',#6930,#6931,#4148,.T.);
#8601=EDGE_CURVE('',#6931,#6931,#5763,.T.);
#8602=EDGE_CURVE('',#6932,#6932,#5764,.T.);
#8603=EDGE_CURVE('',#6932,#6933,#4149,.T.);
#8604=EDGE_CURVE('',#6933,#6933,#5765,.T.);
#8605=EDGE_CURVE('',#6934,#6935,#4150,.T.);
#8606=EDGE_CURVE('',#6934,#6935,#5766,.T.);
#8607=EDGE_CURVE('',#6936,#6934,#619,.T.);
#8608=EDGE_CURVE('',#6937,#6936,#5767,.T.);
#8609=EDGE_CURVE('',#6937,#6938,#4151,.T.);
#8610=EDGE_CURVE('',#6939,#6938,#620,.T.);
#8611=EDGE_CURVE('',#6938,#6939,#621,.T.);
#8612=EDGE_CURVE('',#6940,#6937,#5768,.T.);
#8613=EDGE_CURVE('',#6935,#6940,#622,.T.);
#8614=EDGE_CURVE('',#6940,#6936,#4152,.T.);
#8615=EDGE_CURVE('',#6941,#6941,#5769,.T.);
#8616=EDGE_CURVE('',#6941,#6942,#4153,.T.);
#8617=EDGE_CURVE('',#6942,#6942,#5770,.T.);
#8618=EDGE_CURVE('',#6943,#6943,#5771,.T.);
#8619=EDGE_CURVE('',#6943,#6944,#4154,.T.);
#8620=EDGE_CURVE('',#6944,#6944,#5772,.T.);
#8621=EDGE_CURVE('',#6945,#6946,#623,.T.);
#8622=EDGE_CURVE('',#6947,#6945,#624,.T.);
#8623=EDGE_CURVE('',#6946,#6947,#625,.T.);
#8624=EDGE_CURVE('',#6946,#6948,#4155,.T.);
#8625=EDGE_CURVE('',#6949,#6948,#626,.T.);
#8626=EDGE_CURVE('',#6950,#6949,#627,.T.);
#8627=EDGE_CURVE('',#6951,#6950,#628,.T.);
#8628=EDGE_CURVE('',#6948,#6951,#629,.T.);
#8629=EDGE_CURVE('',#6952,#6953,#630,.T.);
#8630=EDGE_CURVE('',#6953,#6952,#631,.T.);
#8631=EDGE_CURVE('',#6953,#6954,#4156,.T.);
#8632=EDGE_CURVE('',#6955,#6954,#632,.T.);
#8633=EDGE_CURVE('',#6956,#6955,#633,.T.);
#8634=EDGE_CURVE('',#6954,#6956,#634,.T.);
#8635=EDGE_CURVE('',#6957,#6957,#5773,.T.);
#8636=EDGE_CURVE('',#6957,#6947,#4157,.T.);
#8637=EDGE_CURVE('',#6945,#6958,#4158,.T.);
#8638=EDGE_CURVE('',#6958,#6958,#5774,.T.);
#8639=EDGE_CURVE('',#6959,#6960,#635,.T.);
#8640=EDGE_CURVE('',#6960,#6961,#636,.T.);
#8641=EDGE_CURVE('',#6961,#6959,#637,.T.);
#8642=EDGE_CURVE('',#6962,#6963,#638,.T.);
#8643=EDGE_CURVE('',#6963,#6964,#639,.T.);
#8644=EDGE_CURVE('',#6964,#6962,#640,.T.);
#8645=EDGE_CURVE('',#6961,#6965,#4159,.T.);
#8646=EDGE_CURVE('',#6966,#6965,#641,.T.);
#8647=EDGE_CURVE('',#6965,#6966,#642,.T.);
#8648=EDGE_CURVE('',#6967,#6968,#643,.T.);
#8649=EDGE_CURVE('',#6968,#6967,#644,.T.);
#8650=EDGE_CURVE('',#6968,#6964,#4160,.T.);
#8651=EDGE_CURVE('',#6969,#6969,#5775,.T.);
#8652=EDGE_CURVE('',#6969,#6949,#4161,.T.);
#8653=EDGE_CURVE('',#6951,#6970,#4162,.T.);
#8654=EDGE_CURVE('',#6970,#6970,#5776,.T.);
#8655=EDGE_CURVE('',#6971,#6971,#5777,.T.);
#8656=EDGE_CURVE('',#6972,#6973,#5778,.T.);
#8657=EDGE_CURVE('',#6974,#6973,#5779,.T.);
#8658=EDGE_CURVE('',#6974,#6975,#5780,.T.);
#8659=EDGE_CURVE('',#6976,#6975,#5781,.T.);
#8660=EDGE_CURVE('',#6976,#6977,#5782,.T.);
#8661=EDGE_CURVE('',#6978,#6977,#5783,.T.);
#8662=EDGE_CURVE('',#6978,#6979,#5784,.T.);
#8663=EDGE_CURVE('',#6980,#6979,#5785,.T.);
#8664=EDGE_CURVE('',#6980,#6981,#5786,.T.);
#8665=EDGE_CURVE('',#6982,#6981,#5787,.T.);
#8666=EDGE_CURVE('',#6982,#6983,#5788,.T.);
#8667=EDGE_CURVE('',#6984,#6983,#5789,.T.);
#8668=EDGE_CURVE('',#6984,#6985,#5790,.T.);
#8669=EDGE_CURVE('',#6986,#6985,#5791,.T.);
#8670=EDGE_CURVE('',#6986,#6987,#5792,.T.);
#8671=EDGE_CURVE('',#6988,#6987,#5793,.T.);
#8672=EDGE_CURVE('',#6988,#6989,#5794,.T.);
#8673=EDGE_CURVE('',#6990,#6989,#5795,.T.);
#8674=EDGE_CURVE('',#6990,#6991,#5796,.T.);
#8675=EDGE_CURVE('',#6992,#6991,#5797,.T.);
#8676=EDGE_CURVE('',#6992,#6993,#5798,.T.);
#8677=EDGE_CURVE('',#6994,#6993,#5799,.T.);
#8678=EDGE_CURVE('',#6994,#6995,#5800,.T.);
#8679=EDGE_CURVE('',#6996,#6995,#5801,.T.);
#8680=EDGE_CURVE('',#6996,#6997,#5802,.T.);
#8681=EDGE_CURVE('',#6998,#6997,#5803,.T.);
#8682=EDGE_CURVE('',#6998,#6999,#5804,.T.);
#8683=EDGE_CURVE('',#7000,#6999,#5805,.T.);
#8684=EDGE_CURVE('',#7000,#7001,#5806,.T.);
#8685=EDGE_CURVE('',#7002,#7001,#5807,.T.);
#8686=EDGE_CURVE('',#7002,#7003,#5808,.T.);
#8687=EDGE_CURVE('',#7004,#7003,#5809,.T.);
#8688=EDGE_CURVE('',#7004,#7005,#5810,.T.);
#8689=EDGE_CURVE('',#7006,#7005,#5811,.T.);
#8690=EDGE_CURVE('',#7006,#7007,#5812,.T.);
#8691=EDGE_CURVE('',#7008,#7007,#5813,.T.);
#8692=EDGE_CURVE('',#7008,#7009,#5814,.T.);
#8693=EDGE_CURVE('',#7010,#7009,#5815,.T.);
#8694=EDGE_CURVE('',#7010,#7011,#5816,.T.);
#8695=EDGE_CURVE('',#7012,#7011,#5817,.T.);
#8696=EDGE_CURVE('',#7012,#7013,#5818,.T.);
#8697=EDGE_CURVE('',#7014,#7013,#5819,.T.);
#8698=EDGE_CURVE('',#7014,#7015,#5820,.T.);
#8699=EDGE_CURVE('',#7016,#7015,#5821,.T.);
#8700=EDGE_CURVE('',#7016,#7017,#5822,.T.);
#8701=EDGE_CURVE('',#7018,#7017,#5823,.T.);
#8702=EDGE_CURVE('',#7018,#7019,#5824,.T.);
#8703=EDGE_CURVE('',#7020,#7019,#5825,.T.);
#8704=EDGE_CURVE('',#7020,#7021,#5826,.T.);
#8705=EDGE_CURVE('',#7022,#7021,#5827,.T.);
#8706=EDGE_CURVE('',#7022,#7023,#5828,.T.);
#8707=EDGE_CURVE('',#7024,#7023,#5829,.T.);
#8708=EDGE_CURVE('',#7024,#7025,#5830,.T.);
#8709=EDGE_CURVE('',#7026,#7025,#5831,.T.);
#8710=EDGE_CURVE('',#7026,#7027,#5832,.T.);
#8711=EDGE_CURVE('',#7028,#7027,#5833,.T.);
#8712=EDGE_CURVE('',#7028,#7029,#5834,.T.);
#8713=EDGE_CURVE('',#7030,#7029,#5835,.T.);
#8714=EDGE_CURVE('',#7030,#7031,#5836,.T.);
#8715=EDGE_CURVE('',#7032,#7031,#5837,.T.);
#8716=EDGE_CURVE('',#7032,#7033,#5838,.T.);
#8717=EDGE_CURVE('',#7034,#7033,#5839,.T.);
#8718=EDGE_CURVE('',#7034,#7035,#5840,.T.);
#8719=EDGE_CURVE('',#7036,#7035,#5841,.T.);
#8720=EDGE_CURVE('',#7036,#7037,#5842,.T.);
#8721=EDGE_CURVE('',#7038,#7037,#5843,.T.);
#8722=EDGE_CURVE('',#7038,#7039,#5844,.T.);
#8723=EDGE_CURVE('',#7040,#7039,#5845,.T.);
#8724=EDGE_CURVE('',#7040,#7041,#5846,.T.);
#8725=EDGE_CURVE('',#7042,#7041,#5847,.T.);
#8726=EDGE_CURVE('',#7042,#7043,#5848,.T.);
#8727=EDGE_CURVE('',#7044,#7043,#5849,.T.);
#8728=EDGE_CURVE('',#7044,#7045,#5850,.T.);
#8729=EDGE_CURVE('',#7046,#7045,#5851,.T.);
#8730=EDGE_CURVE('',#7046,#7047,#5852,.T.);
#8731=EDGE_CURVE('',#7048,#7047,#5853,.T.);
#8732=EDGE_CURVE('',#7048,#7049,#5854,.T.);
#8733=EDGE_CURVE('',#7050,#7049,#5855,.T.);
#8734=EDGE_CURVE('',#7050,#7051,#5856,.T.);
#8735=EDGE_CURVE('',#6972,#7051,#5857,.T.);
#8736=EDGE_CURVE('',#7052,#7052,#5858,.T.);
#8737=EDGE_CURVE('',#7052,#6971,#4163,.T.);
#8738=EDGE_CURVE('',#7053,#7053,#5859,.T.);
#8739=EDGE_CURVE('',#7054,#7055,#5860,.T.);
#8740=EDGE_CURVE('',#7055,#7056,#5861,.T.);
#8741=EDGE_CURVE('',#7056,#7057,#5862,.T.);
#8742=EDGE_CURVE('',#7057,#7058,#5863,.T.);
#8743=EDGE_CURVE('',#7058,#7059,#5864,.T.);
#8744=EDGE_CURVE('',#7059,#7060,#5865,.T.);
#8745=EDGE_CURVE('',#7060,#7061,#5866,.T.);
#8746=EDGE_CURVE('',#7061,#7062,#5867,.T.);
#8747=EDGE_CURVE('',#7062,#7063,#5868,.T.);
#8748=EDGE_CURVE('',#7063,#7064,#5869,.T.);
#8749=EDGE_CURVE('',#7064,#7065,#5870,.T.);
#8750=EDGE_CURVE('',#7065,#7066,#5871,.T.);
#8751=EDGE_CURVE('',#7066,#7067,#5872,.T.);
#8752=EDGE_CURVE('',#7067,#7068,#5873,.T.);
#8753=EDGE_CURVE('',#7068,#7069,#5874,.T.);
#8754=EDGE_CURVE('',#7069,#7070,#5875,.T.);
#8755=EDGE_CURVE('',#7070,#7071,#5876,.T.);
#8756=EDGE_CURVE('',#7071,#7072,#5877,.T.);
#8757=EDGE_CURVE('',#7072,#7073,#5878,.T.);
#8758=EDGE_CURVE('',#7073,#7074,#5879,.T.);
#8759=EDGE_CURVE('',#7074,#7075,#5880,.T.);
#8760=EDGE_CURVE('',#7075,#7076,#5881,.T.);
#8761=EDGE_CURVE('',#7076,#7077,#5882,.T.);
#8762=EDGE_CURVE('',#7077,#7078,#5883,.T.);
#8763=EDGE_CURVE('',#7078,#7079,#5884,.T.);
#8764=EDGE_CURVE('',#7079,#7080,#5885,.T.);
#8765=EDGE_CURVE('',#7080,#7081,#5886,.T.);
#8766=EDGE_CURVE('',#7081,#7082,#5887,.T.);
#8767=EDGE_CURVE('',#7082,#7083,#5888,.T.);
#8768=EDGE_CURVE('',#7083,#7084,#5889,.T.);
#8769=EDGE_CURVE('',#7084,#7085,#5890,.T.);
#8770=EDGE_CURVE('',#7085,#7086,#5891,.T.);
#8771=EDGE_CURVE('',#7086,#7087,#5892,.T.);
#8772=EDGE_CURVE('',#7087,#7088,#5893,.T.);
#8773=EDGE_CURVE('',#7088,#7089,#5894,.T.);
#8774=EDGE_CURVE('',#7089,#7090,#5895,.T.);
#8775=EDGE_CURVE('',#7090,#7091,#5896,.T.);
#8776=EDGE_CURVE('',#7091,#7092,#5897,.T.);
#8777=EDGE_CURVE('',#7092,#7093,#5898,.T.);
#8778=EDGE_CURVE('',#7093,#7094,#5899,.T.);
#8779=EDGE_CURVE('',#7094,#7095,#5900,.T.);
#8780=EDGE_CURVE('',#7095,#7096,#5901,.T.);
#8781=EDGE_CURVE('',#7096,#7097,#5902,.T.);
#8782=EDGE_CURVE('',#7097,#7098,#5903,.T.);
#8783=EDGE_CURVE('',#7098,#7099,#5904,.T.);
#8784=EDGE_CURVE('',#7099,#7100,#5905,.T.);
#8785=EDGE_CURVE('',#7100,#7101,#5906,.T.);
#8786=EDGE_CURVE('',#7101,#7102,#5907,.T.);
#8787=EDGE_CURVE('',#7102,#7103,#5908,.T.);
#8788=EDGE_CURVE('',#7103,#7104,#5909,.T.);
#8789=EDGE_CURVE('',#7104,#7105,#5910,.T.);
#8790=EDGE_CURVE('',#7105,#7106,#5911,.T.);
#8791=EDGE_CURVE('',#7106,#7107,#5912,.T.);
#8792=EDGE_CURVE('',#7107,#7108,#5913,.T.);
#8793=EDGE_CURVE('',#7108,#7109,#5914,.T.);
#8794=EDGE_CURVE('',#7109,#7110,#5915,.T.);
#8795=EDGE_CURVE('',#7110,#7111,#5916,.T.);
#8796=EDGE_CURVE('',#7111,#7112,#5917,.T.);
#8797=EDGE_CURVE('',#7112,#7113,#5918,.T.);
#8798=EDGE_CURVE('',#7113,#7114,#5919,.T.);
#8799=EDGE_CURVE('',#7114,#7115,#5920,.T.);
#8800=EDGE_CURVE('',#7115,#7116,#5921,.T.);
#8801=EDGE_CURVE('',#7116,#7117,#5922,.T.);
#8802=EDGE_CURVE('',#7117,#7118,#5923,.T.);
#8803=EDGE_CURVE('',#7118,#7119,#5924,.T.);
#8804=EDGE_CURVE('',#7119,#7120,#5925,.T.);
#8805=EDGE_CURVE('',#7120,#7121,#5926,.T.);
#8806=EDGE_CURVE('',#7121,#7122,#5927,.T.);
#8807=EDGE_CURVE('',#7122,#7123,#5928,.T.);
#8808=EDGE_CURVE('',#7123,#7124,#5929,.T.);
#8809=EDGE_CURVE('',#7124,#7125,#5930,.T.);
#8810=EDGE_CURVE('',#7125,#7126,#5931,.T.);
#8811=EDGE_CURVE('',#7126,#7127,#5932,.T.);
#8812=EDGE_CURVE('',#7127,#7128,#5933,.T.);
#8813=EDGE_CURVE('',#7128,#7129,#5934,.T.);
#8814=EDGE_CURVE('',#7129,#7130,#5935,.T.);
#8815=EDGE_CURVE('',#7130,#7131,#5936,.T.);
#8816=EDGE_CURVE('',#7131,#7132,#5937,.T.);
#8817=EDGE_CURVE('',#7132,#7133,#5938,.T.);
#8818=EDGE_CURVE('',#7133,#7054,#5939,.T.);
#8819=EDGE_CURVE('',#7134,#7134,#5940,.T.);
#8820=EDGE_CURVE('',#7134,#7053,#4164,.T.);
#8821=EDGE_CURVE('',#7055,#6972,#4165,.T.);
#8822=EDGE_CURVE('',#6973,#7054,#4166,.T.);
#8823=EDGE_CURVE('',#7133,#6974,#4167,.T.);
#8824=EDGE_CURVE('',#6975,#7132,#4168,.T.);
#8825=EDGE_CURVE('',#7131,#6976,#4169,.T.);
#8826=EDGE_CURVE('',#6977,#7130,#4170,.T.);
#8827=EDGE_CURVE('',#7129,#6978,#4171,.T.);
#8828=EDGE_CURVE('',#6979,#7128,#4172,.T.);
#8829=EDGE_CURVE('',#7127,#6980,#4173,.T.);
#8830=EDGE_CURVE('',#6981,#7126,#4174,.T.);
#8831=EDGE_CURVE('',#7125,#6982,#4175,.T.);
#8832=EDGE_CURVE('',#6983,#7124,#4176,.T.);
#8833=EDGE_CURVE('',#7123,#6984,#4177,.T.);
#8834=EDGE_CURVE('',#6985,#7122,#4178,.T.);
#8835=EDGE_CURVE('',#7121,#6986,#4179,.T.);
#8836=EDGE_CURVE('',#6987,#7120,#4180,.T.);
#8837=EDGE_CURVE('',#7119,#6988,#4181,.T.);
#8838=EDGE_CURVE('',#6989,#7118,#4182,.T.);
#8839=EDGE_CURVE('',#7117,#6990,#4183,.T.);
#8840=EDGE_CURVE('',#6991,#7116,#4184,.T.);
#8841=EDGE_CURVE('',#7115,#6992,#4185,.T.);
#8842=EDGE_CURVE('',#6993,#7114,#4186,.T.);
#8843=EDGE_CURVE('',#7113,#6994,#4187,.T.);
#8844=EDGE_CURVE('',#6995,#7112,#4188,.T.);
#8845=EDGE_CURVE('',#7111,#6996,#4189,.T.);
#8846=EDGE_CURVE('',#6997,#7110,#4190,.T.);
#8847=EDGE_CURVE('',#7109,#6998,#4191,.T.);
#8848=EDGE_CURVE('',#6999,#7108,#4192,.T.);
#8849=EDGE_CURVE('',#7107,#7000,#4193,.T.);
#8850=EDGE_CURVE('',#7001,#7106,#4194,.T.);
#8851=EDGE_CURVE('',#7105,#7002,#4195,.T.);
#8852=EDGE_CURVE('',#7003,#7104,#4196,.T.);
#8853=EDGE_CURVE('',#7103,#7004,#4197,.T.);
#8854=EDGE_CURVE('',#7005,#7102,#4198,.T.);
#8855=EDGE_CURVE('',#7101,#7006,#4199,.T.);
#8856=EDGE_CURVE('',#7007,#7100,#4200,.T.);
#8857=EDGE_CURVE('',#7099,#7008,#4201,.T.);
#8858=EDGE_CURVE('',#7009,#7098,#4202,.T.);
#8859=EDGE_CURVE('',#7097,#7010,#4203,.T.);
#8860=EDGE_CURVE('',#7011,#7096,#4204,.T.);
#8861=EDGE_CURVE('',#7095,#7012,#4205,.T.);
#8862=EDGE_CURVE('',#7013,#7094,#4206,.T.);
#8863=EDGE_CURVE('',#7093,#7014,#4207,.T.);
#8864=EDGE_CURVE('',#7015,#7092,#4208,.T.);
#8865=EDGE_CURVE('',#7091,#7016,#4209,.T.);
#8866=EDGE_CURVE('',#7017,#7090,#4210,.T.);
#8867=EDGE_CURVE('',#7089,#7018,#4211,.T.);
#8868=EDGE_CURVE('',#7019,#7088,#4212,.T.);
#8869=EDGE_CURVE('',#7087,#7020,#4213,.T.);
#8870=EDGE_CURVE('',#7021,#7086,#4214,.T.);
#8871=EDGE_CURVE('',#7085,#7022,#4215,.T.);
#8872=EDGE_CURVE('',#7023,#7084,#4216,.T.);
#8873=EDGE_CURVE('',#7083,#7024,#4217,.T.);
#8874=EDGE_CURVE('',#7025,#7082,#4218,.T.);
#8875=EDGE_CURVE('',#7081,#7026,#4219,.T.);
#8876=EDGE_CURVE('',#7027,#7080,#4220,.T.);
#8877=EDGE_CURVE('',#7079,#7028,#4221,.T.);
#8878=EDGE_CURVE('',#7029,#7078,#4222,.T.);
#8879=EDGE_CURVE('',#7077,#7030,#4223,.T.);
#8880=EDGE_CURVE('',#7031,#7076,#4224,.T.);
#8881=EDGE_CURVE('',#7075,#7032,#4225,.T.);
#8882=EDGE_CURVE('',#7033,#7074,#4226,.T.);
#8883=EDGE_CURVE('',#7073,#7034,#4227,.T.);
#8884=EDGE_CURVE('',#7035,#7072,#4228,.T.);
#8885=EDGE_CURVE('',#7071,#7036,#4229,.T.);
#8886=EDGE_CURVE('',#7037,#7070,#4230,.T.);
#8887=EDGE_CURVE('',#7069,#7038,#4231,.T.);
#8888=EDGE_CURVE('',#7039,#7068,#4232,.T.);
#8889=EDGE_CURVE('',#7067,#7040,#4233,.T.);
#8890=EDGE_CURVE('',#7041,#7066,#4234,.T.);
#8891=EDGE_CURVE('',#7065,#7042,#4235,.T.);
#8892=EDGE_CURVE('',#7043,#7064,#4236,.T.);
#8893=EDGE_CURVE('',#7063,#7044,#4237,.T.);
#8894=EDGE_CURVE('',#7045,#7062,#4238,.T.);
#8895=EDGE_CURVE('',#7061,#7046,#4239,.T.);
#8896=EDGE_CURVE('',#7047,#7060,#4240,.T.);
#8897=EDGE_CURVE('',#7059,#7048,#4241,.T.);
#8898=EDGE_CURVE('',#7049,#7058,#4242,.T.);
#8899=EDGE_CURVE('',#7051,#7056,#4243,.T.);
#8900=EDGE_CURVE('',#7057,#7050,#4244,.T.);
#8901=EDGE_CURVE('',#7135,#7135,#5941,.T.);
#8902=EDGE_CURVE('',#7136,#7136,#5942,.T.);
#8903=EDGE_CURVE('',#7136,#7135,#4245,.T.);
#8904=EDGE_CURVE('',#7137,#7137,#5943,.T.);
#8905=EDGE_CURVE('',#7137,#7136,#4246,.T.);
#8906=EDGE_CURVE('',#7138,#7138,#5944,.T.);
#8907=EDGE_CURVE('',#7138,#7137,#4247,.T.);
#8908=EDGE_CURVE('',#7139,#7139,#5945,.T.);
#8909=EDGE_CURVE('',#7140,#7140,#5946,.F.);
#8910=EDGE_CURVE('',#7140,#7139,#4248,.T.);
#8911=EDGE_CURVE('',#7141,#7141,#5947,.F.);
#8912=EDGE_CURVE('',#7141,#7140,#4249,.T.);
#8913=EDGE_CURVE('',#7142,#7142,#5948,.T.);
#8914=EDGE_CURVE('',#7142,#7141,#4250,.T.);
#8915=EDGE_CURVE('',#7143,#7144,#4251,.T.);
#8916=EDGE_CURVE('',#7144,#7145,#4252,.T.);
#8917=EDGE_CURVE('',#7145,#7146,#4253,.T.);
#8918=EDGE_CURVE('',#7143,#7146,#4254,.T.);
#8919=EDGE_CURVE('',#7144,#7147,#4255,.T.);
#8920=EDGE_CURVE('',#7147,#7148,#4256,.T.);
#8921=EDGE_CURVE('',#7148,#7145,#4257,.T.);
#8922=EDGE_CURVE('',#7147,#7149,#4258,.T.);
#8923=EDGE_CURVE('',#7149,#7150,#4259,.T.);
#8924=EDGE_CURVE('',#7150,#7148,#4260,.T.);
#8925=EDGE_CURVE('',#7149,#7151,#4261,.T.);
#8926=EDGE_CURVE('',#7151,#7152,#4262,.T.);
#8927=EDGE_CURVE('',#7152,#7150,#4263,.T.);
#8928=EDGE_CURVE('',#7151,#7153,#4264,.T.);
#8929=EDGE_CURVE('',#7153,#7154,#4265,.T.);
#8930=EDGE_CURVE('',#7154,#7152,#4266,.T.);
#8931=EDGE_CURVE('',#7153,#7143,#4267,.T.);
#8932=EDGE_CURVE('',#7146,#7154,#4268,.T.);
#8933=EDGE_CURVE('',#7155,#7156,#4269,.T.);
#8934=EDGE_CURVE('',#7155,#7157,#4270,.T.);
#8935=EDGE_CURVE('',#7157,#7158,#4271,.T.);
#8936=EDGE_CURVE('',#7156,#7158,#4272,.T.);
#8937=EDGE_CURVE('',#7159,#7155,#4273,.T.);
#8938=EDGE_CURVE('',#7159,#7160,#4274,.T.);
#8939=EDGE_CURVE('',#7160,#7157,#4275,.T.);
#8940=EDGE_CURVE('',#7161,#7159,#4276,.T.);
#8941=EDGE_CURVE('',#7161,#7162,#4277,.T.);
#8942=EDGE_CURVE('',#7162,#7160,#4278,.T.);
#8943=EDGE_CURVE('',#7163,#7161,#4279,.T.);
#8944=EDGE_CURVE('',#7163,#7164,#4280,.T.);
#8945=EDGE_CURVE('',#7164,#7162,#4281,.T.);
#8946=EDGE_CURVE('',#7165,#7163,#4282,.T.);
#8947=EDGE_CURVE('',#7165,#7166,#4283,.T.);
#8948=EDGE_CURVE('',#7166,#7164,#4284,.T.);
#8949=EDGE_CURVE('',#7156,#7165,#4285,.T.);
#8950=EDGE_CURVE('',#7158,#7166,#4286,.T.);
#8951=EDGE_CURVE('',#7167,#7167,#5949,.T.);
#8952=EDGE_CURVE('',#7168,#7168,#5950,.T.);
#8953=EDGE_CURVE('',#7168,#7167,#4287,.T.);
#8954=EDGE_CURVE('',#7169,#7169,#5951,.F.);
#8955=EDGE_CURVE('',#7169,#7168,#4288,.T.);
#8956=EDGE_CURVE('',#7170,#7170,#5952,.T.);
#8957=EDGE_CURVE('',#7170,#7169,#4289,.T.);
#8958=ORIENTED_EDGE('',*,*,#7171,.F.);
#8959=ORIENTED_EDGE('',*,*,#7172,.T.);
#8960=ORIENTED_EDGE('',*,*,#7173,.F.);
#8961=ORIENTED_EDGE('',*,*,#7172,.F.);
#8962=ORIENTED_EDGE('',*,*,#7171,.T.);
#8963=ORIENTED_EDGE('',*,*,#7174,.F.);
#8964=ORIENTED_EDGE('',*,*,#7175,.T.);
#8965=ORIENTED_EDGE('',*,*,#7176,.F.);
#8966=ORIENTED_EDGE('',*,*,#7175,.F.);
#8967=ORIENTED_EDGE('',*,*,#7174,.T.);
#8968=ORIENTED_EDGE('',*,*,#7177,.F.);
#8969=ORIENTED_EDGE('',*,*,#7178,.T.);
#8970=ORIENTED_EDGE('',*,*,#7179,.F.);
#8971=ORIENTED_EDGE('',*,*,#7178,.F.);
#8972=ORIENTED_EDGE('',*,*,#7177,.T.);
#8973=ORIENTED_EDGE('',*,*,#7180,.F.);
#8974=ORIENTED_EDGE('',*,*,#7181,.T.);
#8975=ORIENTED_EDGE('',*,*,#7182,.F.);
#8976=ORIENTED_EDGE('',*,*,#7181,.F.);
#8977=ORIENTED_EDGE('',*,*,#7180,.T.);
#8978=ORIENTED_EDGE('',*,*,#7183,.F.);
#8979=ORIENTED_EDGE('',*,*,#7184,.T.);
#8980=ORIENTED_EDGE('',*,*,#7185,.F.);
#8981=ORIENTED_EDGE('',*,*,#7184,.F.);
#8982=ORIENTED_EDGE('',*,*,#7183,.T.);
#8983=ORIENTED_EDGE('',*,*,#7186,.F.);
#8984=ORIENTED_EDGE('',*,*,#7187,.T.);
#8985=ORIENTED_EDGE('',*,*,#7188,.F.);
#8986=ORIENTED_EDGE('',*,*,#7187,.F.);
#8987=ORIENTED_EDGE('',*,*,#7186,.T.);
#8988=ORIENTED_EDGE('',*,*,#7189,.F.);
#8989=ORIENTED_EDGE('',*,*,#7190,.T.);
#8990=ORIENTED_EDGE('',*,*,#7191,.F.);
#8991=ORIENTED_EDGE('',*,*,#7190,.F.);
#8992=ORIENTED_EDGE('',*,*,#7189,.T.);
#8993=ORIENTED_EDGE('',*,*,#7192,.F.);
#8994=ORIENTED_EDGE('',*,*,#7193,.T.);
#8995=ORIENTED_EDGE('',*,*,#7194,.F.);
#8996=ORIENTED_EDGE('',*,*,#7193,.F.);
#8997=ORIENTED_EDGE('',*,*,#7192,.T.);
#8998=ORIENTED_EDGE('',*,*,#7195,.F.);
#8999=ORIENTED_EDGE('',*,*,#7196,.T.);
#9000=ORIENTED_EDGE('',*,*,#7197,.F.);
#9001=ORIENTED_EDGE('',*,*,#7196,.F.);
#9002=ORIENTED_EDGE('',*,*,#7195,.T.);
#9003=ORIENTED_EDGE('',*,*,#7198,.F.);
#9004=ORIENTED_EDGE('',*,*,#7199,.T.);
#9005=ORIENTED_EDGE('',*,*,#7200,.F.);
#9006=ORIENTED_EDGE('',*,*,#7199,.F.);
#9007=ORIENTED_EDGE('',*,*,#7198,.T.);
#9008=ORIENTED_EDGE('',*,*,#7201,.F.);
#9009=ORIENTED_EDGE('',*,*,#7202,.F.);
#9010=ORIENTED_EDGE('',*,*,#7203,.T.);
#9011=ORIENTED_EDGE('',*,*,#7204,.F.);
#9012=ORIENTED_EDGE('',*,*,#7205,.T.);
#9013=ORIENTED_EDGE('',*,*,#7206,.F.);
#9014=ORIENTED_EDGE('',*,*,#7207,.F.);
#9015=ORIENTED_EDGE('',*,*,#7208,.F.);
#9016=ORIENTED_EDGE('',*,*,#7209,.F.);
#9017=ORIENTED_EDGE('',*,*,#7210,.F.);
#9018=ORIENTED_EDGE('',*,*,#7211,.F.);
#9019=ORIENTED_EDGE('',*,*,#7212,.F.);
#9020=ORIENTED_EDGE('',*,*,#7213,.T.);
#9021=ORIENTED_EDGE('',*,*,#7214,.T.);
#9022=ORIENTED_EDGE('',*,*,#7215,.T.);
#9023=ORIENTED_EDGE('',*,*,#7216,.T.);
#9024=ORIENTED_EDGE('',*,*,#7217,.T.);
#9025=ORIENTED_EDGE('',*,*,#7218,.T.);
#9026=ORIENTED_EDGE('',*,*,#7219,.T.);
#9027=ORIENTED_EDGE('',*,*,#7220,.T.);
#9028=ORIENTED_EDGE('',*,*,#7221,.T.);
#9029=ORIENTED_EDGE('',*,*,#7222,.T.);
#9030=ORIENTED_EDGE('',*,*,#7223,.T.);
#9031=ORIENTED_EDGE('',*,*,#7224,.T.);
#9032=ORIENTED_EDGE('',*,*,#7202,.T.);
#9033=ORIENTED_EDGE('',*,*,#7225,.T.);
#9034=ORIENTED_EDGE('',*,*,#7208,.T.);
#9035=ORIENTED_EDGE('',*,*,#7226,.T.);
#9036=ORIENTED_EDGE('',*,*,#7227,.F.);
#9037=ORIENTED_EDGE('',*,*,#7203,.F.);
#9038=ORIENTED_EDGE('',*,*,#7226,.F.);
#9039=ORIENTED_EDGE('',*,*,#7207,.T.);
#9040=ORIENTED_EDGE('',*,*,#7225,.F.);
#9041=ORIENTED_EDGE('',*,*,#7201,.T.);
#9042=ORIENTED_EDGE('',*,*,#7228,.F.);
#9043=ORIENTED_EDGE('',*,*,#7205,.F.);
#9044=ORIENTED_EDGE('',*,*,#7229,.F.);
#9045=ORIENTED_EDGE('',*,*,#7213,.F.);
#9046=ORIENTED_EDGE('',*,*,#7230,.T.);
#9047=ORIENTED_EDGE('',*,*,#7231,.F.);
#9048=ORIENTED_EDGE('',*,*,#7232,.T.);
#9049=ORIENTED_EDGE('',*,*,#7233,.F.);
#9050=ORIENTED_EDGE('',*,*,#7234,.F.);
#9051=ORIENTED_EDGE('',*,*,#7215,.F.);
#9052=ORIENTED_EDGE('',*,*,#7235,.F.);
#9053=ORIENTED_EDGE('',*,*,#7230,.F.);
#9054=ORIENTED_EDGE('',*,*,#7216,.F.);
#9055=ORIENTED_EDGE('',*,*,#7234,.T.);
#9056=ORIENTED_EDGE('',*,*,#7214,.F.);
#9057=ORIENTED_EDGE('',*,*,#7229,.T.);
#9058=ORIENTED_EDGE('',*,*,#7236,.F.);
#9059=ORIENTED_EDGE('',*,*,#7232,.F.);
#9060=ORIENTED_EDGE('',*,*,#7237,.F.);
#9061=ORIENTED_EDGE('',*,*,#7238,.F.);
#9062=ORIENTED_EDGE('',*,*,#7239,.F.);
#9063=ORIENTED_EDGE('',*,*,#7221,.F.);
#9064=ORIENTED_EDGE('',*,*,#7240,.T.);
#9065=ORIENTED_EDGE('',*,*,#7241,.F.);
#9066=ORIENTED_EDGE('',*,*,#7242,.F.);
#9067=ORIENTED_EDGE('',*,*,#7243,.F.);
#9068=ORIENTED_EDGE('',*,*,#7244,.T.);
#9069=ORIENTED_EDGE('',*,*,#7245,.F.);
#9070=ORIENTED_EDGE('',*,*,#7246,.F.);
#9071=ORIENTED_EDGE('',*,*,#7223,.F.);
#9072=ORIENTED_EDGE('',*,*,#7247,.F.);
#9073=ORIENTED_EDGE('',*,*,#7240,.F.);
#9074=ORIENTED_EDGE('',*,*,#7224,.F.);
#9075=ORIENTED_EDGE('',*,*,#7246,.T.);
#9076=ORIENTED_EDGE('',*,*,#7222,.F.);
#9077=ORIENTED_EDGE('',*,*,#7239,.T.);
#9078=ORIENTED_EDGE('',*,*,#7248,.F.);
#9079=ORIENTED_EDGE('',*,*,#7244,.F.);
#9080=ORIENTED_EDGE('',*,*,#7249,.F.);
#9081=ORIENTED_EDGE('',*,*,#7250,.F.);
#9082=ORIENTED_EDGE('',*,*,#7251,.F.);
#9083=ORIENTED_EDGE('',*,*,#7217,.F.);
#9084=ORIENTED_EDGE('',*,*,#7252,.T.);
#9085=ORIENTED_EDGE('',*,*,#7253,.F.);
#9086=ORIENTED_EDGE('',*,*,#7254,.F.);
#9087=ORIENTED_EDGE('',*,*,#7255,.F.);
#9088=ORIENTED_EDGE('',*,*,#7256,.T.);
#9089=ORIENTED_EDGE('',*,*,#7257,.F.);
#9090=ORIENTED_EDGE('',*,*,#7258,.F.);
#9091=ORIENTED_EDGE('',*,*,#7219,.F.);
#9092=ORIENTED_EDGE('',*,*,#7259,.F.);
#9093=ORIENTED_EDGE('',*,*,#7252,.F.);
#9094=ORIENTED_EDGE('',*,*,#7220,.F.);
#9095=ORIENTED_EDGE('',*,*,#7258,.T.);
#9096=ORIENTED_EDGE('',*,*,#7218,.F.);
#9097=ORIENTED_EDGE('',*,*,#7251,.T.);
#9098=ORIENTED_EDGE('',*,*,#7260,.F.);
#9099=ORIENTED_EDGE('',*,*,#7256,.F.);
#9100=ORIENTED_EDGE('',*,*,#7254,.T.);
#9101=ORIENTED_EDGE('',*,*,#7261,.F.);
#9102=ORIENTED_EDGE('',*,*,#7249,.T.);
#9103=ORIENTED_EDGE('',*,*,#7262,.F.);
#9104=ORIENTED_EDGE('',*,*,#7255,.T.);
#9105=ORIENTED_EDGE('',*,*,#7262,.T.);
#9106=ORIENTED_EDGE('',*,*,#7263,.F.);
#9107=ORIENTED_EDGE('',*,*,#7264,.T.);
#9108=ORIENTED_EDGE('',*,*,#7265,.F.);
#9109=ORIENTED_EDGE('',*,*,#7264,.F.);
#9110=ORIENTED_EDGE('',*,*,#7263,.T.);
#9111=ORIENTED_EDGE('',*,*,#7266,.F.);
#9112=ORIENTED_EDGE('',*,*,#7267,.T.);
#9113=ORIENTED_EDGE('',*,*,#7268,.F.);
#9114=ORIENTED_EDGE('',*,*,#7267,.F.);
#9115=ORIENTED_EDGE('',*,*,#7266,.T.);
#9116=ORIENTED_EDGE('',*,*,#7242,.T.);
#9117=ORIENTED_EDGE('',*,*,#7269,.F.);
#9118=ORIENTED_EDGE('',*,*,#7237,.T.);
#9119=ORIENTED_EDGE('',*,*,#7270,.F.);
#9120=ORIENTED_EDGE('',*,*,#7243,.T.);
#9121=ORIENTED_EDGE('',*,*,#7270,.T.);
#9122=ORIENTED_EDGE('',*,*,#7210,.T.);
#9123=ORIENTED_EDGE('',*,*,#7271,.T.);
#9124=ORIENTED_EDGE('',*,*,#7272,.F.);
#9125=ORIENTED_EDGE('',*,*,#7273,.F.);
#9126=ORIENTED_EDGE('',*,*,#7211,.T.);
#9127=ORIENTED_EDGE('',*,*,#7273,.T.);
#9128=ORIENTED_EDGE('',*,*,#7274,.F.);
#9129=ORIENTED_EDGE('',*,*,#7275,.F.);
#9130=ORIENTED_EDGE('',*,*,#7212,.T.);
#9131=ORIENTED_EDGE('',*,*,#7275,.T.);
#9132=ORIENTED_EDGE('',*,*,#7276,.F.);
#9133=ORIENTED_EDGE('',*,*,#7277,.F.);
#9134=ORIENTED_EDGE('',*,*,#7209,.T.);
#9135=ORIENTED_EDGE('',*,*,#7277,.T.);
#9136=ORIENTED_EDGE('',*,*,#7278,.F.);
#9137=ORIENTED_EDGE('',*,*,#7271,.F.);
#9138=ORIENTED_EDGE('',*,*,#7278,.T.);
#9139=ORIENTED_EDGE('',*,*,#7276,.T.);
#9140=ORIENTED_EDGE('',*,*,#7274,.T.);
#9141=ORIENTED_EDGE('',*,*,#7272,.T.);
#9142=ORIENTED_EDGE('',*,*,#7176,.T.);
#9143=ORIENTED_EDGE('',*,*,#7182,.T.);
#9144=ORIENTED_EDGE('',*,*,#7188,.T.);
#9145=ORIENTED_EDGE('',*,*,#7194,.T.);
#9146=ORIENTED_EDGE('',*,*,#7268,.T.);
#9147=ORIENTED_EDGE('',*,*,#7265,.T.);
#9148=ORIENTED_EDGE('',*,*,#7253,.T.);
#9149=ORIENTED_EDGE('',*,*,#7259,.T.);
#9150=ORIENTED_EDGE('',*,*,#7257,.T.);
#9151=ORIENTED_EDGE('',*,*,#7260,.T.);
#9152=ORIENTED_EDGE('',*,*,#7250,.T.);
#9153=ORIENTED_EDGE('',*,*,#7261,.T.);
#9154=ORIENTED_EDGE('',*,*,#7241,.T.);
#9155=ORIENTED_EDGE('',*,*,#7247,.T.);
#9156=ORIENTED_EDGE('',*,*,#7245,.T.);
#9157=ORIENTED_EDGE('',*,*,#7248,.T.);
#9158=ORIENTED_EDGE('',*,*,#7238,.T.);
#9159=ORIENTED_EDGE('',*,*,#7269,.T.);
#9160=ORIENTED_EDGE('',*,*,#7231,.T.);
#9161=ORIENTED_EDGE('',*,*,#7235,.T.);
#9162=ORIENTED_EDGE('',*,*,#7233,.T.);
#9163=ORIENTED_EDGE('',*,*,#7236,.T.);
#9164=ORIENTED_EDGE('',*,*,#7204,.T.);
#9165=ORIENTED_EDGE('',*,*,#7227,.T.);
#9166=ORIENTED_EDGE('',*,*,#7206,.T.);
#9167=ORIENTED_EDGE('',*,*,#7228,.T.);
#9168=ORIENTED_EDGE('',*,*,#7200,.T.);
#9169=ORIENTED_EDGE('',*,*,#7197,.T.);
#9170=ORIENTED_EDGE('',*,*,#7191,.T.);
#9171=ORIENTED_EDGE('',*,*,#7185,.T.);
#9172=ORIENTED_EDGE('',*,*,#7179,.T.);
#9173=ORIENTED_EDGE('',*,*,#7173,.T.);
#9174=ORIENTED_EDGE('',*,*,#7279,.T.);
#9175=ORIENTED_EDGE('',*,*,#7280,.T.);
#9176=ORIENTED_EDGE('',*,*,#7281,.F.);
#9177=ORIENTED_EDGE('',*,*,#7282,.F.);
#9178=ORIENTED_EDGE('',*,*,#7283,.T.);
#9179=ORIENTED_EDGE('',*,*,#7282,.T.);
#9180=ORIENTED_EDGE('',*,*,#7284,.F.);
#9181=ORIENTED_EDGE('',*,*,#7285,.F.);
#9182=ORIENTED_EDGE('',*,*,#7286,.T.);
#9183=ORIENTED_EDGE('',*,*,#7285,.T.);
#9184=ORIENTED_EDGE('',*,*,#7287,.F.);
#9185=ORIENTED_EDGE('',*,*,#7288,.F.);
#9186=ORIENTED_EDGE('',*,*,#7289,.T.);
#9187=ORIENTED_EDGE('',*,*,#7288,.T.);
#9188=ORIENTED_EDGE('',*,*,#7290,.F.);
#9189=ORIENTED_EDGE('',*,*,#7280,.F.);
#9190=ORIENTED_EDGE('',*,*,#7290,.T.);
#9191=ORIENTED_EDGE('',*,*,#7287,.T.);
#9192=ORIENTED_EDGE('',*,*,#7284,.T.);
#9193=ORIENTED_EDGE('',*,*,#7281,.T.);
#9194=ORIENTED_EDGE('',*,*,#7289,.F.);
#9195=ORIENTED_EDGE('',*,*,#7279,.F.);
#9196=ORIENTED_EDGE('',*,*,#7283,.F.);
#9197=ORIENTED_EDGE('',*,*,#7286,.F.);
#9198=ORIENTED_EDGE('',*,*,#7291,.T.);
#9199=ORIENTED_EDGE('',*,*,#7292,.T.);
#9200=ORIENTED_EDGE('',*,*,#7293,.F.);
#9201=ORIENTED_EDGE('',*,*,#7294,.F.);
#9202=ORIENTED_EDGE('',*,*,#7295,.T.);
#9203=ORIENTED_EDGE('',*,*,#7294,.T.);
#9204=ORIENTED_EDGE('',*,*,#7296,.F.);
#9205=ORIENTED_EDGE('',*,*,#7297,.F.);
#9206=ORIENTED_EDGE('',*,*,#7298,.T.);
#9207=ORIENTED_EDGE('',*,*,#7297,.T.);
#9208=ORIENTED_EDGE('',*,*,#7299,.F.);
#9209=ORIENTED_EDGE('',*,*,#7300,.F.);
#9210=ORIENTED_EDGE('',*,*,#7301,.T.);
#9211=ORIENTED_EDGE('',*,*,#7300,.T.);
#9212=ORIENTED_EDGE('',*,*,#7302,.F.);
#9213=ORIENTED_EDGE('',*,*,#7292,.F.);
#9214=ORIENTED_EDGE('',*,*,#7302,.T.);
#9215=ORIENTED_EDGE('',*,*,#7299,.T.);
#9216=ORIENTED_EDGE('',*,*,#7296,.T.);
#9217=ORIENTED_EDGE('',*,*,#7293,.T.);
#9218=ORIENTED_EDGE('',*,*,#7301,.F.);
#9219=ORIENTED_EDGE('',*,*,#7291,.F.);
#9220=ORIENTED_EDGE('',*,*,#7295,.F.);
#9221=ORIENTED_EDGE('',*,*,#7298,.F.);
#9222=ORIENTED_EDGE('',*,*,#7303,.F.);
#9223=ORIENTED_EDGE('',*,*,#7304,.T.);
#9224=ORIENTED_EDGE('',*,*,#7305,.F.);
#9225=ORIENTED_EDGE('',*,*,#7304,.F.);
#9226=ORIENTED_EDGE('',*,*,#7306,.F.);
#9227=ORIENTED_EDGE('',*,*,#7307,.T.);
#9228=ORIENTED_EDGE('',*,*,#7308,.F.);
#9229=ORIENTED_EDGE('',*,*,#7307,.F.);
#9230=ORIENTED_EDGE('',*,*,#7309,.F.);
#9231=ORIENTED_EDGE('',*,*,#7310,.T.);
#9232=ORIENTED_EDGE('',*,*,#7311,.F.);
#9233=ORIENTED_EDGE('',*,*,#7310,.F.);
#9234=ORIENTED_EDGE('',*,*,#7312,.F.);
#9235=ORIENTED_EDGE('',*,*,#7313,.T.);
#9236=ORIENTED_EDGE('',*,*,#7314,.F.);
#9237=ORIENTED_EDGE('',*,*,#7313,.F.);
#9238=ORIENTED_EDGE('',*,*,#7315,.F.);
#9239=ORIENTED_EDGE('',*,*,#7316,.T.);
#9240=ORIENTED_EDGE('',*,*,#7317,.F.);
#9241=ORIENTED_EDGE('',*,*,#7316,.F.);
#9242=ORIENTED_EDGE('',*,*,#7318,.F.);
#9243=ORIENTED_EDGE('',*,*,#7319,.T.);
#9244=ORIENTED_EDGE('',*,*,#7320,.F.);
#9245=ORIENTED_EDGE('',*,*,#7319,.F.);
#9246=ORIENTED_EDGE('',*,*,#7321,.F.);
#9247=ORIENTED_EDGE('',*,*,#7322,.T.);
#9248=ORIENTED_EDGE('',*,*,#7323,.F.);
#9249=ORIENTED_EDGE('',*,*,#7322,.F.);
#9250=ORIENTED_EDGE('',*,*,#7324,.F.);
#9251=ORIENTED_EDGE('',*,*,#7325,.T.);
#9252=ORIENTED_EDGE('',*,*,#7326,.F.);
#9253=ORIENTED_EDGE('',*,*,#7325,.F.);
#9254=ORIENTED_EDGE('',*,*,#7327,.F.);
#9255=ORIENTED_EDGE('',*,*,#7328,.T.);
#9256=ORIENTED_EDGE('',*,*,#7329,.F.);
#9257=ORIENTED_EDGE('',*,*,#7328,.F.);
#9258=ORIENTED_EDGE('',*,*,#7330,.F.);
#9259=ORIENTED_EDGE('',*,*,#7331,.F.);
#9260=ORIENTED_EDGE('',*,*,#7332,.T.);
#9261=ORIENTED_EDGE('',*,*,#7333,.F.);
#9262=ORIENTED_EDGE('',*,*,#7320,.T.);
#9263=ORIENTED_EDGE('',*,*,#7329,.T.);
#9264=ORIENTED_EDGE('',*,*,#7334,.F.);
#9265=ORIENTED_EDGE('',*,*,#7335,.F.);
#9266=ORIENTED_EDGE('',*,*,#7336,.F.);
#9267=ORIENTED_EDGE('',*,*,#7337,.F.);
#9268=ORIENTED_EDGE('',*,*,#7323,.T.);
#9269=ORIENTED_EDGE('',*,*,#7326,.T.);
#9270=ORIENTED_EDGE('',*,*,#7338,.F.);
#9271=ORIENTED_EDGE('',*,*,#7336,.T.);
#9272=ORIENTED_EDGE('',*,*,#7339,.F.);
#9273=ORIENTED_EDGE('',*,*,#7340,.F.);
#9274=ORIENTED_EDGE('',*,*,#7341,.F.);
#9275=ORIENTED_EDGE('',*,*,#7342,.T.);
#9276=ORIENTED_EDGE('',*,*,#7343,.F.);
#9277=ORIENTED_EDGE('',*,*,#7332,.F.);
#9278=ORIENTED_EDGE('',*,*,#7344,.T.);
#9279=ORIENTED_EDGE('',*,*,#7345,.F.);
#9280=ORIENTED_EDGE('',*,*,#7346,.F.);
#9281=ORIENTED_EDGE('',*,*,#7337,.T.);
#9282=ORIENTED_EDGE('',*,*,#7338,.T.);
#9283=ORIENTED_EDGE('',*,*,#7347,.T.);
#9284=ORIENTED_EDGE('',*,*,#7341,.T.);
#9285=ORIENTED_EDGE('',*,*,#7331,.T.);
#9286=ORIENTED_EDGE('',*,*,#7315,.T.);
#9287=ORIENTED_EDGE('',*,*,#7312,.T.);
#9288=ORIENTED_EDGE('',*,*,#7309,.T.);
#9289=ORIENTED_EDGE('',*,*,#7306,.T.);
#9290=ORIENTED_EDGE('',*,*,#7303,.T.);
#9291=ORIENTED_EDGE('',*,*,#7330,.T.);
#9292=ORIENTED_EDGE('',*,*,#7348,.T.);
#9293=ORIENTED_EDGE('',*,*,#7349,.F.);
#9294=ORIENTED_EDGE('',*,*,#7344,.F.);
#9295=ORIENTED_EDGE('',*,*,#7350,.T.);
#9296=ORIENTED_EDGE('',*,*,#7351,.F.);
#9297=ORIENTED_EDGE('',*,*,#7348,.F.);
#9298=ORIENTED_EDGE('',*,*,#7333,.T.);
#9299=ORIENTED_EDGE('',*,*,#7343,.T.);
#9300=ORIENTED_EDGE('',*,*,#7352,.T.);
#9301=ORIENTED_EDGE('',*,*,#7339,.T.);
#9302=ORIENTED_EDGE('',*,*,#7335,.T.);
#9303=ORIENTED_EDGE('',*,*,#7317,.T.);
#9304=ORIENTED_EDGE('',*,*,#7314,.T.);
#9305=ORIENTED_EDGE('',*,*,#7311,.T.);
#9306=ORIENTED_EDGE('',*,*,#7308,.T.);
#9307=ORIENTED_EDGE('',*,*,#7305,.T.);
#9308=ORIENTED_EDGE('',*,*,#7334,.T.);
#9309=ORIENTED_EDGE('',*,*,#7346,.T.);
#9310=ORIENTED_EDGE('',*,*,#7353,.F.);
#9311=ORIENTED_EDGE('',*,*,#7350,.F.);
#9312=ORIENTED_EDGE('',*,*,#7353,.T.);
#9313=ORIENTED_EDGE('',*,*,#7345,.T.);
#9314=ORIENTED_EDGE('',*,*,#7349,.T.);
#9315=ORIENTED_EDGE('',*,*,#7351,.T.);
#9316=ORIENTED_EDGE('',*,*,#7352,.F.);
#9317=ORIENTED_EDGE('',*,*,#7342,.F.);
#9318=ORIENTED_EDGE('',*,*,#7347,.F.);
#9319=ORIENTED_EDGE('',*,*,#7340,.T.);
#9320=ORIENTED_EDGE('',*,*,#7318,.T.);
#9321=ORIENTED_EDGE('',*,*,#7321,.T.);
#9322=ORIENTED_EDGE('',*,*,#7324,.T.);
#9323=ORIENTED_EDGE('',*,*,#7327,.T.);
#9324=ORIENTED_EDGE('',*,*,#7354,.F.);
#9325=ORIENTED_EDGE('',*,*,#7355,.T.);
#9326=ORIENTED_EDGE('',*,*,#7356,.T.);
#9327=ORIENTED_EDGE('',*,*,#7355,.F.);
#9328=ORIENTED_EDGE('',*,*,#7357,.F.);
#9329=ORIENTED_EDGE('',*,*,#7358,.T.);
#9330=ORIENTED_EDGE('',*,*,#7359,.T.);
#9331=ORIENTED_EDGE('',*,*,#7358,.F.);
#9332=ORIENTED_EDGE('',*,*,#7357,.T.);
#9333=ORIENTED_EDGE('',*,*,#7354,.T.);
#9334=ORIENTED_EDGE('',*,*,#7359,.F.);
#9335=ORIENTED_EDGE('',*,*,#7356,.F.);
#9336=ORIENTED_EDGE('',*,*,#7360,.F.);
#9337=ORIENTED_EDGE('',*,*,#7361,.F.);
#9338=ORIENTED_EDGE('',*,*,#7362,.F.);
#9339=ORIENTED_EDGE('',*,*,#7363,.F.);
#9340=ORIENTED_EDGE('',*,*,#7364,.F.);
#9341=ORIENTED_EDGE('',*,*,#7365,.F.);
#9342=ORIENTED_EDGE('',*,*,#7366,.F.);
#9343=ORIENTED_EDGE('',*,*,#7367,.F.);
#9344=ORIENTED_EDGE('',*,*,#7368,.F.);
#9345=ORIENTED_EDGE('',*,*,#7369,.F.);
#9346=ORIENTED_EDGE('',*,*,#7370,.F.);
#9347=ORIENTED_EDGE('',*,*,#7371,.F.);
#9348=ORIENTED_EDGE('',*,*,#7372,.F.);
#9349=ORIENTED_EDGE('',*,*,#7373,.F.);
#9350=ORIENTED_EDGE('',*,*,#7374,.F.);
#9351=ORIENTED_EDGE('',*,*,#7375,.F.);
#9352=ORIENTED_EDGE('',*,*,#7361,.T.);
#9353=ORIENTED_EDGE('',*,*,#7376,.F.);
#9354=ORIENTED_EDGE('',*,*,#7373,.T.);
#9355=ORIENTED_EDGE('',*,*,#7377,.F.);
#9356=ORIENTED_EDGE('',*,*,#7369,.T.);
#9357=ORIENTED_EDGE('',*,*,#7378,.F.);
#9358=ORIENTED_EDGE('',*,*,#7365,.T.);
#9359=ORIENTED_EDGE('',*,*,#7379,.F.);
#9360=ORIENTED_EDGE('',*,*,#7380,.F.);
#9361=ORIENTED_EDGE('',*,*,#7370,.T.);
#9362=ORIENTED_EDGE('',*,*,#7377,.T.);
#9363=ORIENTED_EDGE('',*,*,#7372,.T.);
#9364=ORIENTED_EDGE('',*,*,#7381,.F.);
#9365=ORIENTED_EDGE('',*,*,#7366,.T.);
#9366=ORIENTED_EDGE('',*,*,#7378,.T.);
#9367=ORIENTED_EDGE('',*,*,#7368,.T.);
#9368=ORIENTED_EDGE('',*,*,#7382,.F.);
#9369=ORIENTED_EDGE('',*,*,#7360,.T.);
#9370=ORIENTED_EDGE('',*,*,#7383,.F.);
#9371=ORIENTED_EDGE('',*,*,#7374,.T.);
#9372=ORIENTED_EDGE('',*,*,#7376,.T.);
#9373=ORIENTED_EDGE('',*,*,#7362,.T.);
#9374=ORIENTED_EDGE('',*,*,#7379,.T.);
#9375=ORIENTED_EDGE('',*,*,#7364,.T.);
#9376=ORIENTED_EDGE('',*,*,#7384,.F.);
#9377=ORIENTED_EDGE('',*,*,#7385,.F.);
#9378=ORIENTED_EDGE('',*,*,#7386,.T.);
#9379=ORIENTED_EDGE('',*,*,#7387,.F.);
#9380=ORIENTED_EDGE('',*,*,#7386,.F.);
#9381=ORIENTED_EDGE('',*,*,#7385,.T.);
#9382=ORIENTED_EDGE('',*,*,#7388,.T.);
#9383=ORIENTED_EDGE('',*,*,#7388,.F.);
#9384=ORIENTED_EDGE('',*,*,#7389,.T.);
#9385=ORIENTED_EDGE('',*,*,#7380,.T.);
#9386=ORIENTED_EDGE('',*,*,#7389,.F.);
#9387=ORIENTED_EDGE('',*,*,#7363,.T.);
#9388=ORIENTED_EDGE('',*,*,#7384,.T.);
#9389=ORIENTED_EDGE('',*,*,#7367,.T.);
#9390=ORIENTED_EDGE('',*,*,#7382,.T.);
#9391=ORIENTED_EDGE('',*,*,#7371,.T.);
#9392=ORIENTED_EDGE('',*,*,#7381,.T.);
#9393=ORIENTED_EDGE('',*,*,#7375,.T.);
#9394=ORIENTED_EDGE('',*,*,#7383,.T.);
#9395=ORIENTED_EDGE('',*,*,#7387,.T.);
#9396=ORIENTED_EDGE('',*,*,#7390,.F.);
#9397=ORIENTED_EDGE('',*,*,#7391,.F.);
#9398=ORIENTED_EDGE('',*,*,#7392,.F.);
#9399=ORIENTED_EDGE('',*,*,#7393,.F.);
#9400=ORIENTED_EDGE('',*,*,#7394,.F.);
#9401=ORIENTED_EDGE('',*,*,#7395,.F.);
#9402=ORIENTED_EDGE('',*,*,#7396,.F.);
#9403=ORIENTED_EDGE('',*,*,#7397,.F.);
#9404=ORIENTED_EDGE('',*,*,#7398,.F.);
#9405=ORIENTED_EDGE('',*,*,#7399,.F.);
#9406=ORIENTED_EDGE('',*,*,#7400,.F.);
#9407=ORIENTED_EDGE('',*,*,#7401,.F.);
#9408=ORIENTED_EDGE('',*,*,#7402,.F.);
#9409=ORIENTED_EDGE('',*,*,#7403,.F.);
#9410=ORIENTED_EDGE('',*,*,#7404,.F.);
#9411=ORIENTED_EDGE('',*,*,#7405,.F.);
#9412=ORIENTED_EDGE('',*,*,#7391,.T.);
#9413=ORIENTED_EDGE('',*,*,#7406,.F.);
#9414=ORIENTED_EDGE('',*,*,#7403,.T.);
#9415=ORIENTED_EDGE('',*,*,#7407,.F.);
#9416=ORIENTED_EDGE('',*,*,#7399,.T.);
#9417=ORIENTED_EDGE('',*,*,#7408,.F.);
#9418=ORIENTED_EDGE('',*,*,#7395,.T.);
#9419=ORIENTED_EDGE('',*,*,#7409,.F.);
#9420=ORIENTED_EDGE('',*,*,#7410,.T.);
#9421=ORIENTED_EDGE('',*,*,#7400,.T.);
#9422=ORIENTED_EDGE('',*,*,#7407,.T.);
#9423=ORIENTED_EDGE('',*,*,#7402,.T.);
#9424=ORIENTED_EDGE('',*,*,#7411,.F.);
#9425=ORIENTED_EDGE('',*,*,#7396,.T.);
#9426=ORIENTED_EDGE('',*,*,#7408,.T.);
#9427=ORIENTED_EDGE('',*,*,#7398,.T.);
#9428=ORIENTED_EDGE('',*,*,#7412,.F.);
#9429=ORIENTED_EDGE('',*,*,#7390,.T.);
#9430=ORIENTED_EDGE('',*,*,#7413,.F.);
#9431=ORIENTED_EDGE('',*,*,#7404,.T.);
#9432=ORIENTED_EDGE('',*,*,#7406,.T.);
#9433=ORIENTED_EDGE('',*,*,#7392,.T.);
#9434=ORIENTED_EDGE('',*,*,#7409,.T.);
#9435=ORIENTED_EDGE('',*,*,#7394,.T.);
#9436=ORIENTED_EDGE('',*,*,#7414,.F.);
#9437=ORIENTED_EDGE('',*,*,#7410,.F.);
#9438=ORIENTED_EDGE('',*,*,#7415,.T.);
#9439=ORIENTED_EDGE('',*,*,#7416,.T.);
#9440=ORIENTED_EDGE('',*,*,#7415,.F.);
#9441=ORIENTED_EDGE('',*,*,#7416,.F.);
#9442=ORIENTED_EDGE('',*,*,#7417,.F.);
#9443=ORIENTED_EDGE('',*,*,#7418,.F.);
#9444=ORIENTED_EDGE('',*,*,#7419,.T.);
#9445=ORIENTED_EDGE('',*,*,#7417,.T.);
#9446=ORIENTED_EDGE('',*,*,#7419,.F.);
#9447=ORIENTED_EDGE('',*,*,#7393,.T.);
#9448=ORIENTED_EDGE('',*,*,#7414,.T.);
#9449=ORIENTED_EDGE('',*,*,#7397,.T.);
#9450=ORIENTED_EDGE('',*,*,#7412,.T.);
#9451=ORIENTED_EDGE('',*,*,#7401,.T.);
#9452=ORIENTED_EDGE('',*,*,#7411,.T.);
#9453=ORIENTED_EDGE('',*,*,#7405,.T.);
#9454=ORIENTED_EDGE('',*,*,#7413,.T.);
#9455=ORIENTED_EDGE('',*,*,#7418,.T.);
#9456=ORIENTED_EDGE('',*,*,#7420,.F.);
#9457=ORIENTED_EDGE('',*,*,#7421,.F.);
#9458=ORIENTED_EDGE('',*,*,#7422,.F.);
#9459=ORIENTED_EDGE('',*,*,#7423,.F.);
#9460=ORIENTED_EDGE('',*,*,#7424,.F.);
#9461=ORIENTED_EDGE('',*,*,#7425,.F.);
#9462=ORIENTED_EDGE('',*,*,#7426,.F.);
#9463=ORIENTED_EDGE('',*,*,#7427,.F.);
#9464=ORIENTED_EDGE('',*,*,#7428,.F.);
#9465=ORIENTED_EDGE('',*,*,#7429,.T.);
#9466=ORIENTED_EDGE('',*,*,#7430,.F.);
#9467=ORIENTED_EDGE('',*,*,#7427,.T.);
#9468=ORIENTED_EDGE('',*,*,#7431,.F.);
#9469=ORIENTED_EDGE('',*,*,#7421,.T.);
#9470=ORIENTED_EDGE('',*,*,#7432,.F.);
#9471=ORIENTED_EDGE('',*,*,#7433,.F.);
#9472=ORIENTED_EDGE('',*,*,#7434,.F.);
#9473=ORIENTED_EDGE('',*,*,#7435,.F.);
#9474=ORIENTED_EDGE('',*,*,#7436,.F.);
#9475=ORIENTED_EDGE('',*,*,#7437,.F.);
#9476=ORIENTED_EDGE('',*,*,#7438,.F.);
#9477=ORIENTED_EDGE('',*,*,#7439,.F.);
#9478=ORIENTED_EDGE('',*,*,#7429,.F.);
#9479=ORIENTED_EDGE('',*,*,#7437,.T.);
#9480=ORIENTED_EDGE('',*,*,#7428,.T.);
#9481=ORIENTED_EDGE('',*,*,#7420,.T.);
#9482=ORIENTED_EDGE('',*,*,#7440,.T.);
#9483=ORIENTED_EDGE('',*,*,#7441,.F.);
#9484=ORIENTED_EDGE('',*,*,#7442,.F.);
#9485=ORIENTED_EDGE('',*,*,#7443,.T.);
#9486=ORIENTED_EDGE('',*,*,#7444,.T.);
#9487=ORIENTED_EDGE('',*,*,#7422,.T.);
#9488=ORIENTED_EDGE('',*,*,#7431,.T.);
#9489=ORIENTED_EDGE('',*,*,#7426,.T.);
#9490=ORIENTED_EDGE('',*,*,#7445,.T.);
#9491=ORIENTED_EDGE('',*,*,#7446,.T.);
#9492=ORIENTED_EDGE('',*,*,#7447,.T.);
#9493=ORIENTED_EDGE('',*,*,#7441,.T.);
#9494=ORIENTED_EDGE('',*,*,#7448,.T.);
#9495=ORIENTED_EDGE('',*,*,#7423,.T.);
#9496=ORIENTED_EDGE('',*,*,#7448,.F.);
#9497=ORIENTED_EDGE('',*,*,#7440,.F.);
#9498=ORIENTED_EDGE('',*,*,#7425,.T.);
#9499=ORIENTED_EDGE('',*,*,#7449,.T.);
#9500=ORIENTED_EDGE('',*,*,#7445,.F.);
#9501=ORIENTED_EDGE('',*,*,#7450,.F.);
#9502=ORIENTED_EDGE('',*,*,#7451,.T.);
#9503=ORIENTED_EDGE('',*,*,#7436,.T.);
#9504=ORIENTED_EDGE('',*,*,#7451,.F.);
#9505=ORIENTED_EDGE('',*,*,#7452,.F.);
#9506=ORIENTED_EDGE('',*,*,#7453,.T.);
#9507=ORIENTED_EDGE('',*,*,#7435,.T.);
#9508=ORIENTED_EDGE('',*,*,#7453,.F.);
#9509=ORIENTED_EDGE('',*,*,#7454,.F.);
#9510=ORIENTED_EDGE('',*,*,#7455,.T.);
#9511=ORIENTED_EDGE('',*,*,#7434,.T.);
#9512=ORIENTED_EDGE('',*,*,#7455,.F.);
#9513=ORIENTED_EDGE('',*,*,#7456,.F.);
#9514=ORIENTED_EDGE('',*,*,#7457,.T.);
#9515=ORIENTED_EDGE('',*,*,#7433,.T.);
#9516=ORIENTED_EDGE('',*,*,#7457,.F.);
#9517=ORIENTED_EDGE('',*,*,#7458,.F.);
#9518=ORIENTED_EDGE('',*,*,#7459,.T.);
#9519=ORIENTED_EDGE('',*,*,#7432,.T.);
#9520=ORIENTED_EDGE('',*,*,#7459,.F.);
#9521=ORIENTED_EDGE('',*,*,#7460,.F.);
#9522=ORIENTED_EDGE('',*,*,#7461,.T.);
#9523=ORIENTED_EDGE('',*,*,#7462,.F.);
#9524=ORIENTED_EDGE('',*,*,#7461,.F.);
#9525=ORIENTED_EDGE('',*,*,#7463,.F.);
#9526=ORIENTED_EDGE('',*,*,#7464,.T.);
#9527=ORIENTED_EDGE('',*,*,#7465,.F.);
#9528=ORIENTED_EDGE('',*,*,#7464,.F.);
#9529=ORIENTED_EDGE('',*,*,#7466,.F.);
#9530=ORIENTED_EDGE('',*,*,#7467,.T.);
#9531=ORIENTED_EDGE('',*,*,#7468,.F.);
#9532=ORIENTED_EDGE('',*,*,#7467,.F.);
#9533=ORIENTED_EDGE('',*,*,#7469,.F.);
#9534=ORIENTED_EDGE('',*,*,#7470,.T.);
#9535=ORIENTED_EDGE('',*,*,#7471,.F.);
#9536=ORIENTED_EDGE('',*,*,#7470,.F.);
#9537=ORIENTED_EDGE('',*,*,#7443,.F.);
#9538=ORIENTED_EDGE('',*,*,#7472,.F.);
#9539=ORIENTED_EDGE('',*,*,#7473,.T.);
#9540=ORIENTED_EDGE('',*,*,#7474,.F.);
#9541=ORIENTED_EDGE('',*,*,#7462,.T.);
#9542=ORIENTED_EDGE('',*,*,#7471,.T.);
#9543=ORIENTED_EDGE('',*,*,#7475,.F.);
#9544=ORIENTED_EDGE('',*,*,#7476,.F.);
#9545=ORIENTED_EDGE('',*,*,#7477,.F.);
#9546=ORIENTED_EDGE('',*,*,#7478,.F.);
#9547=ORIENTED_EDGE('',*,*,#7465,.T.);
#9548=ORIENTED_EDGE('',*,*,#7468,.T.);
#9549=ORIENTED_EDGE('',*,*,#7479,.F.);
#9550=ORIENTED_EDGE('',*,*,#7477,.T.);
#9551=ORIENTED_EDGE('',*,*,#7480,.F.);
#9552=ORIENTED_EDGE('',*,*,#7481,.F.);
#9553=ORIENTED_EDGE('',*,*,#7482,.F.);
#9554=ORIENTED_EDGE('',*,*,#7483,.T.);
#9555=ORIENTED_EDGE('',*,*,#7484,.F.);
#9556=ORIENTED_EDGE('',*,*,#7473,.F.);
#9557=ORIENTED_EDGE('',*,*,#7442,.T.);
#9558=ORIENTED_EDGE('',*,*,#7447,.F.);
#9559=ORIENTED_EDGE('',*,*,#7485,.F.);
#9560=ORIENTED_EDGE('',*,*,#7478,.T.);
#9561=ORIENTED_EDGE('',*,*,#7479,.T.);
#9562=ORIENTED_EDGE('',*,*,#7486,.T.);
#9563=ORIENTED_EDGE('',*,*,#7482,.T.);
#9564=ORIENTED_EDGE('',*,*,#7472,.T.);
#9565=ORIENTED_EDGE('',*,*,#7458,.T.);
#9566=ORIENTED_EDGE('',*,*,#7456,.T.);
#9567=ORIENTED_EDGE('',*,*,#7454,.T.);
#9568=ORIENTED_EDGE('',*,*,#7452,.T.);
#9569=ORIENTED_EDGE('',*,*,#7450,.T.);
#9570=ORIENTED_EDGE('',*,*,#7438,.T.);
#9571=ORIENTED_EDGE('',*,*,#7444,.F.);
#9572=ORIENTED_EDGE('',*,*,#7474,.T.);
#9573=ORIENTED_EDGE('',*,*,#7484,.T.);
#9574=ORIENTED_EDGE('',*,*,#7487,.T.);
#9575=ORIENTED_EDGE('',*,*,#7480,.T.);
#9576=ORIENTED_EDGE('',*,*,#7476,.T.);
#9577=ORIENTED_EDGE('',*,*,#7488,.T.);
#9578=ORIENTED_EDGE('',*,*,#7439,.T.);
#9579=ORIENTED_EDGE('',*,*,#7488,.F.);
#9580=ORIENTED_EDGE('',*,*,#7475,.T.);
#9581=ORIENTED_EDGE('',*,*,#7485,.T.);
#9582=ORIENTED_EDGE('',*,*,#7446,.F.);
#9583=ORIENTED_EDGE('',*,*,#7449,.F.);
#9584=ORIENTED_EDGE('',*,*,#7424,.T.);
#9585=ORIENTED_EDGE('',*,*,#7430,.T.);
#9586=ORIENTED_EDGE('',*,*,#7487,.F.);
#9587=ORIENTED_EDGE('',*,*,#7483,.F.);
#9588=ORIENTED_EDGE('',*,*,#7486,.F.);
#9589=ORIENTED_EDGE('',*,*,#7481,.T.);
#9590=ORIENTED_EDGE('',*,*,#7460,.T.);
#9591=ORIENTED_EDGE('',*,*,#7463,.T.);
#9592=ORIENTED_EDGE('',*,*,#7466,.T.);
#9593=ORIENTED_EDGE('',*,*,#7469,.T.);
#9594=ORIENTED_EDGE('',*,*,#7489,.F.);
#9595=ORIENTED_EDGE('',*,*,#7490,.T.);
#9596=ORIENTED_EDGE('',*,*,#7491,.T.);
#9597=ORIENTED_EDGE('',*,*,#7490,.F.);
#9598=ORIENTED_EDGE('',*,*,#7492,.F.);
#9599=ORIENTED_EDGE('',*,*,#7493,.T.);
#9600=ORIENTED_EDGE('',*,*,#7494,.T.);
#9601=ORIENTED_EDGE('',*,*,#7493,.F.);
#9602=ORIENTED_EDGE('',*,*,#7492,.T.);
#9603=ORIENTED_EDGE('',*,*,#7489,.T.);
#9604=ORIENTED_EDGE('',*,*,#7494,.F.);
#9605=ORIENTED_EDGE('',*,*,#7491,.F.);
#9606=ORIENTED_EDGE('',*,*,#7495,.F.);
#9607=ORIENTED_EDGE('',*,*,#7496,.T.);
#9608=ORIENTED_EDGE('',*,*,#7497,.T.);
#9609=ORIENTED_EDGE('',*,*,#7496,.F.);
#9610=ORIENTED_EDGE('',*,*,#7498,.F.);
#9611=ORIENTED_EDGE('',*,*,#7499,.T.);
#9612=ORIENTED_EDGE('',*,*,#7500,.T.);
#9613=ORIENTED_EDGE('',*,*,#7499,.F.);
#9614=ORIENTED_EDGE('',*,*,#7498,.T.);
#9615=ORIENTED_EDGE('',*,*,#7495,.T.);
#9616=ORIENTED_EDGE('',*,*,#7500,.F.);
#9617=ORIENTED_EDGE('',*,*,#7497,.F.);
#9618=ORIENTED_EDGE('',*,*,#7501,.F.);
#9619=ORIENTED_EDGE('',*,*,#7502,.T.);
#9620=ORIENTED_EDGE('',*,*,#7503,.T.);
#9621=ORIENTED_EDGE('',*,*,#7502,.F.);
#9622=ORIENTED_EDGE('',*,*,#7504,.F.);
#9623=ORIENTED_EDGE('',*,*,#7505,.T.);
#9624=ORIENTED_EDGE('',*,*,#7506,.T.);
#9625=ORIENTED_EDGE('',*,*,#7505,.F.);
#9626=ORIENTED_EDGE('',*,*,#7504,.T.);
#9627=ORIENTED_EDGE('',*,*,#7501,.T.);
#9628=ORIENTED_EDGE('',*,*,#7506,.F.);
#9629=ORIENTED_EDGE('',*,*,#7503,.F.);
#9630=ORIENTED_EDGE('',*,*,#7507,.F.);
#9631=ORIENTED_EDGE('',*,*,#7508,.T.);
#9632=ORIENTED_EDGE('',*,*,#7509,.T.);
#9633=ORIENTED_EDGE('',*,*,#7508,.F.);
#9634=ORIENTED_EDGE('',*,*,#7510,.F.);
#9635=ORIENTED_EDGE('',*,*,#7511,.T.);
#9636=ORIENTED_EDGE('',*,*,#7512,.T.);
#9637=ORIENTED_EDGE('',*,*,#7511,.F.);
#9638=ORIENTED_EDGE('',*,*,#7510,.T.);
#9639=ORIENTED_EDGE('',*,*,#7507,.T.);
#9640=ORIENTED_EDGE('',*,*,#7512,.F.);
#9641=ORIENTED_EDGE('',*,*,#7509,.F.);
#9642=ORIENTED_EDGE('',*,*,#7513,.F.);
#9643=ORIENTED_EDGE('',*,*,#7514,.T.);
#9644=ORIENTED_EDGE('',*,*,#7515,.T.);
#9645=ORIENTED_EDGE('',*,*,#7514,.F.);
#9646=ORIENTED_EDGE('',*,*,#7516,.F.);
#9647=ORIENTED_EDGE('',*,*,#7517,.T.);
#9648=ORIENTED_EDGE('',*,*,#7518,.T.);
#9649=ORIENTED_EDGE('',*,*,#7517,.F.);
#9650=ORIENTED_EDGE('',*,*,#7516,.T.);
#9651=ORIENTED_EDGE('',*,*,#7513,.T.);
#9652=ORIENTED_EDGE('',*,*,#7518,.F.);
#9653=ORIENTED_EDGE('',*,*,#7515,.F.);
#9654=ORIENTED_EDGE('',*,*,#7519,.F.);
#9655=ORIENTED_EDGE('',*,*,#7520,.F.);
#9656=ORIENTED_EDGE('',*,*,#7521,.F.);
#9657=ORIENTED_EDGE('',*,*,#7522,.F.);
#9658=ORIENTED_EDGE('',*,*,#7523,.F.);
#9659=ORIENTED_EDGE('',*,*,#7524,.F.);
#9660=ORIENTED_EDGE('',*,*,#7525,.F.);
#9661=ORIENTED_EDGE('',*,*,#7526,.F.);
#9662=ORIENTED_EDGE('',*,*,#7527,.F.);
#9663=ORIENTED_EDGE('',*,*,#7528,.F.);
#9664=ORIENTED_EDGE('',*,*,#7529,.F.);
#9665=ORIENTED_EDGE('',*,*,#7530,.F.);
#9666=ORIENTED_EDGE('',*,*,#7531,.F.);
#9667=ORIENTED_EDGE('',*,*,#7532,.F.);
#9668=ORIENTED_EDGE('',*,*,#7533,.F.);
#9669=ORIENTED_EDGE('',*,*,#7534,.F.);
#9670=ORIENTED_EDGE('',*,*,#7520,.T.);
#9671=ORIENTED_EDGE('',*,*,#7535,.F.);
#9672=ORIENTED_EDGE('',*,*,#7532,.T.);
#9673=ORIENTED_EDGE('',*,*,#7536,.F.);
#9674=ORIENTED_EDGE('',*,*,#7528,.T.);
#9675=ORIENTED_EDGE('',*,*,#7537,.F.);
#9676=ORIENTED_EDGE('',*,*,#7524,.T.);
#9677=ORIENTED_EDGE('',*,*,#7538,.F.);
#9678=ORIENTED_EDGE('',*,*,#7539,.F.);
#9679=ORIENTED_EDGE('',*,*,#7529,.T.);
#9680=ORIENTED_EDGE('',*,*,#7536,.T.);
#9681=ORIENTED_EDGE('',*,*,#7531,.T.);
#9682=ORIENTED_EDGE('',*,*,#7540,.F.);
#9683=ORIENTED_EDGE('',*,*,#7525,.T.);
#9684=ORIENTED_EDGE('',*,*,#7537,.T.);
#9685=ORIENTED_EDGE('',*,*,#7527,.T.);
#9686=ORIENTED_EDGE('',*,*,#7541,.F.);
#9687=ORIENTED_EDGE('',*,*,#7519,.T.);
#9688=ORIENTED_EDGE('',*,*,#7542,.F.);
#9689=ORIENTED_EDGE('',*,*,#7533,.T.);
#9690=ORIENTED_EDGE('',*,*,#7535,.T.);
#9691=ORIENTED_EDGE('',*,*,#7521,.T.);
#9692=ORIENTED_EDGE('',*,*,#7538,.T.);
#9693=ORIENTED_EDGE('',*,*,#7523,.T.);
#9694=ORIENTED_EDGE('',*,*,#7543,.F.);
#9695=ORIENTED_EDGE('',*,*,#7544,.F.);
#9696=ORIENTED_EDGE('',*,*,#7545,.T.);
#9697=ORIENTED_EDGE('',*,*,#7546,.F.);
#9698=ORIENTED_EDGE('',*,*,#7545,.F.);
#9699=ORIENTED_EDGE('',*,*,#7544,.T.);
#9700=ORIENTED_EDGE('',*,*,#7547,.T.);
#9701=ORIENTED_EDGE('',*,*,#7547,.F.);
#9702=ORIENTED_EDGE('',*,*,#7548,.T.);
#9703=ORIENTED_EDGE('',*,*,#7539,.T.);
#9704=ORIENTED_EDGE('',*,*,#7548,.F.);
#9705=ORIENTED_EDGE('',*,*,#7522,.T.);
#9706=ORIENTED_EDGE('',*,*,#7543,.T.);
#9707=ORIENTED_EDGE('',*,*,#7526,.T.);
#9708=ORIENTED_EDGE('',*,*,#7541,.T.);
#9709=ORIENTED_EDGE('',*,*,#7530,.T.);
#9710=ORIENTED_EDGE('',*,*,#7540,.T.);
#9711=ORIENTED_EDGE('',*,*,#7534,.T.);
#9712=ORIENTED_EDGE('',*,*,#7542,.T.);
#9713=ORIENTED_EDGE('',*,*,#7546,.T.);
#9714=ORIENTED_EDGE('',*,*,#7549,.F.);
#9715=ORIENTED_EDGE('',*,*,#7550,.F.);
#9716=ORIENTED_EDGE('',*,*,#7551,.F.);
#9717=ORIENTED_EDGE('',*,*,#7552,.F.);
#9718=ORIENTED_EDGE('',*,*,#7553,.F.);
#9719=ORIENTED_EDGE('',*,*,#7554,.F.);
#9720=ORIENTED_EDGE('',*,*,#7555,.F.);
#9721=ORIENTED_EDGE('',*,*,#7550,.T.);
#9722=ORIENTED_EDGE('',*,*,#7556,.F.);
#9723=ORIENTED_EDGE('',*,*,#7557,.T.);
#9724=ORIENTED_EDGE('',*,*,#7558,.F.);
#9725=ORIENTED_EDGE('',*,*,#7559,.F.);
#9726=ORIENTED_EDGE('',*,*,#7560,.F.);
#9727=ORIENTED_EDGE('',*,*,#7561,.F.);
#9728=ORIENTED_EDGE('',*,*,#7562,.F.);
#9729=ORIENTED_EDGE('',*,*,#7557,.F.);
#9730=ORIENTED_EDGE('',*,*,#7563,.F.);
#9731=ORIENTED_EDGE('',*,*,#7564,.T.);
#9732=ORIENTED_EDGE('',*,*,#7565,.F.);
#9733=ORIENTED_EDGE('',*,*,#7566,.F.);
#9734=ORIENTED_EDGE('',*,*,#7567,.F.);
#9735=ORIENTED_EDGE('',*,*,#7568,.F.);
#9736=ORIENTED_EDGE('',*,*,#7569,.F.);
#9737=ORIENTED_EDGE('',*,*,#7564,.F.);
#9738=ORIENTED_EDGE('',*,*,#7570,.F.);
#9739=ORIENTED_EDGE('',*,*,#7571,.T.);
#9740=ORIENTED_EDGE('',*,*,#7572,.F.);
#9741=ORIENTED_EDGE('',*,*,#7573,.F.);
#9742=ORIENTED_EDGE('',*,*,#7574,.F.);
#9743=ORIENTED_EDGE('',*,*,#7575,.F.);
#9744=ORIENTED_EDGE('',*,*,#7576,.F.);
#9745=ORIENTED_EDGE('',*,*,#7571,.F.);
#9746=ORIENTED_EDGE('',*,*,#7559,.T.);
#9747=ORIENTED_EDGE('',*,*,#7577,.F.);
#9748=ORIENTED_EDGE('',*,*,#7578,.F.);
#9749=ORIENTED_EDGE('',*,*,#7579,.F.);
#9750=ORIENTED_EDGE('',*,*,#7566,.T.);
#9751=ORIENTED_EDGE('',*,*,#7580,.F.);
#9752=ORIENTED_EDGE('',*,*,#7581,.F.);
#9753=ORIENTED_EDGE('',*,*,#7582,.F.);
#9754=ORIENTED_EDGE('',*,*,#7573,.T.);
#9755=ORIENTED_EDGE('',*,*,#7583,.F.);
#9756=ORIENTED_EDGE('',*,*,#7584,.F.);
#9757=ORIENTED_EDGE('',*,*,#7585,.F.);
#9758=ORIENTED_EDGE('',*,*,#7553,.T.);
#9759=ORIENTED_EDGE('',*,*,#7549,.T.);
#9760=ORIENTED_EDGE('',*,*,#7586,.F.);
#9761=ORIENTED_EDGE('',*,*,#7574,.T.);
#9762=ORIENTED_EDGE('',*,*,#7570,.T.);
#9763=ORIENTED_EDGE('',*,*,#7585,.T.);
#9764=ORIENTED_EDGE('',*,*,#7587,.T.);
#9765=ORIENTED_EDGE('',*,*,#7588,.T.);
#9766=ORIENTED_EDGE('',*,*,#7552,.T.);
#9767=ORIENTED_EDGE('',*,*,#7589,.T.);
#9768=ORIENTED_EDGE('',*,*,#7561,.T.);
#9769=ORIENTED_EDGE('',*,*,#7590,.T.);
#9770=ORIENTED_EDGE('',*,*,#7568,.T.);
#9771=ORIENTED_EDGE('',*,*,#7591,.T.);
#9772=ORIENTED_EDGE('',*,*,#7575,.T.);
#9773=ORIENTED_EDGE('',*,*,#7586,.T.);
#9774=ORIENTED_EDGE('',*,*,#7592,.T.);
#9775=ORIENTED_EDGE('',*,*,#7593,.T.);
#9776=ORIENTED_EDGE('',*,*,#7587,.F.);
#9777=ORIENTED_EDGE('',*,*,#7584,.T.);
#9778=ORIENTED_EDGE('',*,*,#7594,.F.);
#9779=ORIENTED_EDGE('',*,*,#7581,.T.);
#9780=ORIENTED_EDGE('',*,*,#7595,.F.);
#9781=ORIENTED_EDGE('',*,*,#7578,.T.);
#9782=ORIENTED_EDGE('',*,*,#7596,.F.);
#9783=ORIENTED_EDGE('',*,*,#7597,.F.);
#9784=ORIENTED_EDGE('',*,*,#7563,.T.);
#9785=ORIENTED_EDGE('',*,*,#7582,.T.);
#9786=ORIENTED_EDGE('',*,*,#7594,.T.);
#9787=ORIENTED_EDGE('',*,*,#7583,.T.);
#9788=ORIENTED_EDGE('',*,*,#7572,.T.);
#9789=ORIENTED_EDGE('',*,*,#7576,.T.);
#9790=ORIENTED_EDGE('',*,*,#7591,.F.);
#9791=ORIENTED_EDGE('',*,*,#7567,.T.);
#9792=ORIENTED_EDGE('',*,*,#7556,.T.);
#9793=ORIENTED_EDGE('',*,*,#7579,.T.);
#9794=ORIENTED_EDGE('',*,*,#7595,.T.);
#9795=ORIENTED_EDGE('',*,*,#7580,.T.);
#9796=ORIENTED_EDGE('',*,*,#7565,.T.);
#9797=ORIENTED_EDGE('',*,*,#7569,.T.);
#9798=ORIENTED_EDGE('',*,*,#7590,.F.);
#9799=ORIENTED_EDGE('',*,*,#7560,.T.);
#9800=ORIENTED_EDGE('',*,*,#7554,.T.);
#9801=ORIENTED_EDGE('',*,*,#7588,.F.);
#9802=ORIENTED_EDGE('',*,*,#7593,.F.);
#9803=ORIENTED_EDGE('',*,*,#7598,.F.);
#9804=ORIENTED_EDGE('',*,*,#7555,.T.);
#9805=ORIENTED_EDGE('',*,*,#7598,.T.);
#9806=ORIENTED_EDGE('',*,*,#7596,.T.);
#9807=ORIENTED_EDGE('',*,*,#7577,.T.);
#9808=ORIENTED_EDGE('',*,*,#7558,.T.);
#9809=ORIENTED_EDGE('',*,*,#7562,.T.);
#9810=ORIENTED_EDGE('',*,*,#7589,.F.);
#9811=ORIENTED_EDGE('',*,*,#7551,.T.);
#9812=ORIENTED_EDGE('',*,*,#7592,.F.);
#9813=ORIENTED_EDGE('',*,*,#7599,.T.);
#9814=ORIENTED_EDGE('',*,*,#7597,.T.);
#9815=ORIENTED_EDGE('',*,*,#7599,.F.);
#9816=ORIENTED_EDGE('',*,*,#7600,.F.);
#9817=ORIENTED_EDGE('',*,*,#7601,.F.);
#9818=ORIENTED_EDGE('',*,*,#7602,.F.);
#9819=ORIENTED_EDGE('',*,*,#7603,.T.);
#9820=ORIENTED_EDGE('',*,*,#7604,.F.);
#9821=ORIENTED_EDGE('',*,*,#7605,.F.);
#9822=ORIENTED_EDGE('',*,*,#7606,.F.);
#9823=ORIENTED_EDGE('',*,*,#7607,.F.);
#9824=ORIENTED_EDGE('',*,*,#7608,.F.);
#9825=ORIENTED_EDGE('',*,*,#7609,.F.);
#9826=ORIENTED_EDGE('',*,*,#7610,.F.);
#9827=ORIENTED_EDGE('',*,*,#7611,.F.);
#9828=ORIENTED_EDGE('',*,*,#7600,.T.);
#9829=ORIENTED_EDGE('',*,*,#7612,.T.);
#9830=ORIENTED_EDGE('',*,*,#7604,.T.);
#9831=ORIENTED_EDGE('',*,*,#7613,.T.);
#9832=ORIENTED_EDGE('',*,*,#7603,.F.);
#9833=ORIENTED_EDGE('',*,*,#7614,.F.);
#9834=ORIENTED_EDGE('',*,*,#7605,.T.);
#9835=ORIENTED_EDGE('',*,*,#7612,.F.);
#9836=ORIENTED_EDGE('',*,*,#7601,.T.);
#9837=ORIENTED_EDGE('',*,*,#7613,.F.);
#9838=ORIENTED_EDGE('',*,*,#7607,.T.);
#9839=ORIENTED_EDGE('',*,*,#7615,.F.);
#9840=ORIENTED_EDGE('',*,*,#7616,.T.);
#9841=ORIENTED_EDGE('',*,*,#7617,.F.);
#9842=ORIENTED_EDGE('',*,*,#7618,.F.);
#9843=ORIENTED_EDGE('',*,*,#7611,.T.);
#9844=ORIENTED_EDGE('',*,*,#7610,.T.);
#9845=ORIENTED_EDGE('',*,*,#7619,.T.);
#9846=ORIENTED_EDGE('',*,*,#7620,.F.);
#9847=ORIENTED_EDGE('',*,*,#7616,.F.);
#9848=ORIENTED_EDGE('',*,*,#7608,.T.);
#9849=ORIENTED_EDGE('',*,*,#7618,.T.);
#9850=ORIENTED_EDGE('',*,*,#7621,.F.);
#9851=ORIENTED_EDGE('',*,*,#7622,.F.);
#9852=ORIENTED_EDGE('',*,*,#7619,.F.);
#9853=ORIENTED_EDGE('',*,*,#7609,.T.);
#9854=ORIENTED_EDGE('',*,*,#7622,.T.);
#9855=ORIENTED_EDGE('',*,*,#7623,.F.);
#9856=ORIENTED_EDGE('',*,*,#7620,.T.);
#9857=ORIENTED_EDGE('',*,*,#7623,.T.);
#9858=ORIENTED_EDGE('',*,*,#7621,.T.);
#9859=ORIENTED_EDGE('',*,*,#7617,.T.);
#9860=ORIENTED_EDGE('',*,*,#7602,.T.);
#9861=ORIENTED_EDGE('',*,*,#7615,.T.);
#9862=ORIENTED_EDGE('',*,*,#7606,.T.);
#9863=ORIENTED_EDGE('',*,*,#7614,.T.);
#9864=ORIENTED_EDGE('',*,*,#7624,.F.);
#9865=ORIENTED_EDGE('',*,*,#7625,.T.);
#9866=ORIENTED_EDGE('',*,*,#7626,.F.);
#9867=ORIENTED_EDGE('',*,*,#7625,.F.);
#9868=ORIENTED_EDGE('',*,*,#7624,.T.);
#9869=ORIENTED_EDGE('',*,*,#7627,.F.);
#9870=ORIENTED_EDGE('',*,*,#7628,.F.);
#9871=ORIENTED_EDGE('',*,*,#7629,.T.);
#9872=ORIENTED_EDGE('',*,*,#7627,.T.);
#9873=ORIENTED_EDGE('',*,*,#7629,.F.);
#9874=ORIENTED_EDGE('',*,*,#7630,.F.);
#9875=ORIENTED_EDGE('',*,*,#7631,.T.);
#9876=ORIENTED_EDGE('',*,*,#7632,.F.);
#9877=ORIENTED_EDGE('',*,*,#7631,.F.);
#9878=ORIENTED_EDGE('',*,*,#7630,.T.);
#9879=ORIENTED_EDGE('',*,*,#7633,.F.);
#9880=ORIENTED_EDGE('',*,*,#7634,.F.);
#9881=ORIENTED_EDGE('',*,*,#7635,.T.);
#9882=ORIENTED_EDGE('',*,*,#7633,.T.);
#9883=ORIENTED_EDGE('',*,*,#7635,.F.);
#9884=ORIENTED_EDGE('',*,*,#7636,.F.);
#9885=ORIENTED_EDGE('',*,*,#7637,.T.);
#9886=ORIENTED_EDGE('',*,*,#7638,.F.);
#9887=ORIENTED_EDGE('',*,*,#7637,.F.);
#9888=ORIENTED_EDGE('',*,*,#7636,.T.);
#9889=ORIENTED_EDGE('',*,*,#7639,.F.);
#9890=ORIENTED_EDGE('',*,*,#7640,.F.);
#9891=ORIENTED_EDGE('',*,*,#7641,.T.);
#9892=ORIENTED_EDGE('',*,*,#7639,.T.);
#9893=ORIENTED_EDGE('',*,*,#7641,.F.);
#9894=ORIENTED_EDGE('',*,*,#7642,.F.);
#9895=ORIENTED_EDGE('',*,*,#7643,.T.);
#9896=ORIENTED_EDGE('',*,*,#7644,.F.);
#9897=ORIENTED_EDGE('',*,*,#7643,.F.);
#9898=ORIENTED_EDGE('',*,*,#7642,.T.);
#9899=ORIENTED_EDGE('',*,*,#7645,.F.);
#9900=ORIENTED_EDGE('',*,*,#7646,.F.);
#9901=ORIENTED_EDGE('',*,*,#7647,.T.);
#9902=ORIENTED_EDGE('',*,*,#7645,.T.);
#9903=ORIENTED_EDGE('',*,*,#7647,.F.);
#9904=ORIENTED_EDGE('',*,*,#7648,.F.);
#9905=ORIENTED_EDGE('',*,*,#7649,.T.);
#9906=ORIENTED_EDGE('',*,*,#7650,.F.);
#9907=ORIENTED_EDGE('',*,*,#7649,.F.);
#9908=ORIENTED_EDGE('',*,*,#7648,.T.);
#9909=ORIENTED_EDGE('',*,*,#7651,.F.);
#9910=ORIENTED_EDGE('',*,*,#7652,.T.);
#9911=ORIENTED_EDGE('',*,*,#7653,.F.);
#9912=ORIENTED_EDGE('',*,*,#7652,.F.);
#9913=ORIENTED_EDGE('',*,*,#7651,.T.);
#9914=ORIENTED_EDGE('',*,*,#7654,.T.);
#9915=ORIENTED_EDGE('',*,*,#7655,.T.);
#9916=ORIENTED_EDGE('',*,*,#7656,.F.);
#9917=ORIENTED_EDGE('',*,*,#7657,.F.);
#9918=ORIENTED_EDGE('',*,*,#7658,.T.);
#9919=ORIENTED_EDGE('',*,*,#7657,.T.);
#9920=ORIENTED_EDGE('',*,*,#7659,.F.);
#9921=ORIENTED_EDGE('',*,*,#7660,.F.);
#9922=ORIENTED_EDGE('',*,*,#7661,.T.);
#9923=ORIENTED_EDGE('',*,*,#7660,.T.);
#9924=ORIENTED_EDGE('',*,*,#7662,.F.);
#9925=ORIENTED_EDGE('',*,*,#7663,.F.);
#9926=ORIENTED_EDGE('',*,*,#7664,.T.);
#9927=ORIENTED_EDGE('',*,*,#7663,.T.);
#9928=ORIENTED_EDGE('',*,*,#7665,.F.);
#9929=ORIENTED_EDGE('',*,*,#7655,.F.);
#9930=ORIENTED_EDGE('',*,*,#7665,.T.);
#9931=ORIENTED_EDGE('',*,*,#7662,.T.);
#9932=ORIENTED_EDGE('',*,*,#7659,.T.);
#9933=ORIENTED_EDGE('',*,*,#7656,.T.);
#9934=ORIENTED_EDGE('',*,*,#7626,.T.);
#9935=ORIENTED_EDGE('',*,*,#7632,.T.);
#9936=ORIENTED_EDGE('',*,*,#7638,.T.);
#9937=ORIENTED_EDGE('',*,*,#7644,.T.);
#9938=ORIENTED_EDGE('',*,*,#7650,.T.);
#9939=ORIENTED_EDGE('',*,*,#7653,.T.);
#9940=ORIENTED_EDGE('',*,*,#7664,.F.);
#9941=ORIENTED_EDGE('',*,*,#7654,.F.);
#9942=ORIENTED_EDGE('',*,*,#7658,.F.);
#9943=ORIENTED_EDGE('',*,*,#7661,.F.);
#9944=ORIENTED_EDGE('',*,*,#7628,.T.);
#9945=ORIENTED_EDGE('',*,*,#7634,.T.);
#9946=ORIENTED_EDGE('',*,*,#7640,.T.);
#9947=ORIENTED_EDGE('',*,*,#7646,.T.);
#9948=ORIENTED_EDGE('',*,*,#7666,.F.);
#9949=ORIENTED_EDGE('',*,*,#7667,.T.);
#9950=ORIENTED_EDGE('',*,*,#7668,.T.);
#9951=ORIENTED_EDGE('',*,*,#7667,.F.);
#9952=ORIENTED_EDGE('',*,*,#7669,.F.);
#9953=ORIENTED_EDGE('',*,*,#7670,.T.);
#9954=ORIENTED_EDGE('',*,*,#7671,.T.);
#9955=ORIENTED_EDGE('',*,*,#7670,.F.);
#9956=ORIENTED_EDGE('',*,*,#7669,.T.);
#9957=ORIENTED_EDGE('',*,*,#7666,.T.);
#9958=ORIENTED_EDGE('',*,*,#7671,.F.);
#9959=ORIENTED_EDGE('',*,*,#7668,.F.);
#9960=ORIENTED_EDGE('',*,*,#7672,.F.);
#9961=ORIENTED_EDGE('',*,*,#7673,.T.);
#9962=ORIENTED_EDGE('',*,*,#7674,.T.);
#9963=ORIENTED_EDGE('',*,*,#7673,.F.);
#9964=ORIENTED_EDGE('',*,*,#7675,.F.);
#9965=ORIENTED_EDGE('',*,*,#7676,.T.);
#9966=ORIENTED_EDGE('',*,*,#7677,.T.);
#9967=ORIENTED_EDGE('',*,*,#7676,.F.);
#9968=ORIENTED_EDGE('',*,*,#7675,.T.);
#9969=ORIENTED_EDGE('',*,*,#7672,.T.);
#9970=ORIENTED_EDGE('',*,*,#7677,.F.);
#9971=ORIENTED_EDGE('',*,*,#7674,.F.);
#9972=ORIENTED_EDGE('',*,*,#7678,.F.);
#9973=ORIENTED_EDGE('',*,*,#7679,.T.);
#9974=ORIENTED_EDGE('',*,*,#7680,.F.);
#9975=ORIENTED_EDGE('',*,*,#7679,.F.);
#9976=ORIENTED_EDGE('',*,*,#7678,.T.);
#9977=ORIENTED_EDGE('',*,*,#7681,.F.);
#9978=ORIENTED_EDGE('',*,*,#7682,.F.);
#9979=ORIENTED_EDGE('',*,*,#7683,.T.);
#9980=ORIENTED_EDGE('',*,*,#7681,.T.);
#9981=ORIENTED_EDGE('',*,*,#7683,.F.);
#9982=ORIENTED_EDGE('',*,*,#7684,.F.);
#9983=ORIENTED_EDGE('',*,*,#7685,.T.);
#9984=ORIENTED_EDGE('',*,*,#7686,.F.);
#9985=ORIENTED_EDGE('',*,*,#7685,.F.);
#9986=ORIENTED_EDGE('',*,*,#7684,.T.);
#9987=ORIENTED_EDGE('',*,*,#7687,.F.);
#9988=ORIENTED_EDGE('',*,*,#7688,.F.);
#9989=ORIENTED_EDGE('',*,*,#7689,.T.);
#9990=ORIENTED_EDGE('',*,*,#7687,.T.);
#9991=ORIENTED_EDGE('',*,*,#7689,.F.);
#9992=ORIENTED_EDGE('',*,*,#7690,.F.);
#9993=ORIENTED_EDGE('',*,*,#7691,.T.);
#9994=ORIENTED_EDGE('',*,*,#7692,.F.);
#9995=ORIENTED_EDGE('',*,*,#7691,.F.);
#9996=ORIENTED_EDGE('',*,*,#7690,.T.);
#9997=ORIENTED_EDGE('',*,*,#7693,.F.);
#9998=ORIENTED_EDGE('',*,*,#7694,.F.);
#9999=ORIENTED_EDGE('',*,*,#7695,.T.);
#10000=ORIENTED_EDGE('',*,*,#7693,.T.);
#10001=ORIENTED_EDGE('',*,*,#7695,.F.);
#10002=ORIENTED_EDGE('',*,*,#7696,.F.);
#10003=ORIENTED_EDGE('',*,*,#7697,.T.);
#10004=ORIENTED_EDGE('',*,*,#7698,.F.);
#10005=ORIENTED_EDGE('',*,*,#7697,.F.);
#10006=ORIENTED_EDGE('',*,*,#7696,.T.);
#10007=ORIENTED_EDGE('',*,*,#7699,.F.);
#10008=ORIENTED_EDGE('',*,*,#7700,.F.);
#10009=ORIENTED_EDGE('',*,*,#7701,.T.);
#10010=ORIENTED_EDGE('',*,*,#7699,.T.);
#10011=ORIENTED_EDGE('',*,*,#7701,.F.);
#10012=ORIENTED_EDGE('',*,*,#7702,.F.);
#10013=ORIENTED_EDGE('',*,*,#7703,.T.);
#10014=ORIENTED_EDGE('',*,*,#7704,.F.);
#10015=ORIENTED_EDGE('',*,*,#7703,.F.);
#10016=ORIENTED_EDGE('',*,*,#7702,.T.);
#10017=ORIENTED_EDGE('',*,*,#7705,.F.);
#10018=ORIENTED_EDGE('',*,*,#7706,.T.);
#10019=ORIENTED_EDGE('',*,*,#7707,.F.);
#10020=ORIENTED_EDGE('',*,*,#7706,.F.);
#10021=ORIENTED_EDGE('',*,*,#7705,.T.);
#10022=ORIENTED_EDGE('',*,*,#7708,.T.);
#10023=ORIENTED_EDGE('',*,*,#7709,.T.);
#10024=ORIENTED_EDGE('',*,*,#7710,.F.);
#10025=ORIENTED_EDGE('',*,*,#7711,.F.);
#10026=ORIENTED_EDGE('',*,*,#7712,.T.);
#10027=ORIENTED_EDGE('',*,*,#7711,.T.);
#10028=ORIENTED_EDGE('',*,*,#7713,.F.);
#10029=ORIENTED_EDGE('',*,*,#7714,.F.);
#10030=ORIENTED_EDGE('',*,*,#7715,.T.);
#10031=ORIENTED_EDGE('',*,*,#7714,.T.);
#10032=ORIENTED_EDGE('',*,*,#7716,.F.);
#10033=ORIENTED_EDGE('',*,*,#7717,.F.);
#10034=ORIENTED_EDGE('',*,*,#7718,.T.);
#10035=ORIENTED_EDGE('',*,*,#7717,.T.);
#10036=ORIENTED_EDGE('',*,*,#7719,.F.);
#10037=ORIENTED_EDGE('',*,*,#7709,.F.);
#10038=ORIENTED_EDGE('',*,*,#7719,.T.);
#10039=ORIENTED_EDGE('',*,*,#7716,.T.);
#10040=ORIENTED_EDGE('',*,*,#7713,.T.);
#10041=ORIENTED_EDGE('',*,*,#7710,.T.);
#10042=ORIENTED_EDGE('',*,*,#7680,.T.);
#10043=ORIENTED_EDGE('',*,*,#7686,.T.);
#10044=ORIENTED_EDGE('',*,*,#7692,.T.);
#10045=ORIENTED_EDGE('',*,*,#7698,.T.);
#10046=ORIENTED_EDGE('',*,*,#7704,.T.);
#10047=ORIENTED_EDGE('',*,*,#7707,.T.);
#10048=ORIENTED_EDGE('',*,*,#7718,.F.);
#10049=ORIENTED_EDGE('',*,*,#7708,.F.);
#10050=ORIENTED_EDGE('',*,*,#7712,.F.);
#10051=ORIENTED_EDGE('',*,*,#7715,.F.);
#10052=ORIENTED_EDGE('',*,*,#7682,.T.);
#10053=ORIENTED_EDGE('',*,*,#7688,.T.);
#10054=ORIENTED_EDGE('',*,*,#7694,.T.);
#10055=ORIENTED_EDGE('',*,*,#7700,.T.);
#10056=ORIENTED_EDGE('',*,*,#7720,.F.);
#10057=ORIENTED_EDGE('',*,*,#7721,.T.);
#10058=ORIENTED_EDGE('',*,*,#7722,.T.);
#10059=ORIENTED_EDGE('',*,*,#7721,.F.);
#10060=ORIENTED_EDGE('',*,*,#7723,.F.);
#10061=ORIENTED_EDGE('',*,*,#7724,.T.);
#10062=ORIENTED_EDGE('',*,*,#7725,.T.);
#10063=ORIENTED_EDGE('',*,*,#7724,.F.);
#10064=ORIENTED_EDGE('',*,*,#7723,.T.);
#10065=ORIENTED_EDGE('',*,*,#7720,.T.);
#10066=ORIENTED_EDGE('',*,*,#7725,.F.);
#10067=ORIENTED_EDGE('',*,*,#7722,.F.);
#10068=ORIENTED_EDGE('',*,*,#7726,.F.);
#10069=ORIENTED_EDGE('',*,*,#7727,.T.);
#10070=ORIENTED_EDGE('',*,*,#7728,.T.);
#10071=ORIENTED_EDGE('',*,*,#7727,.F.);
#10072=ORIENTED_EDGE('',*,*,#7729,.F.);
#10073=ORIENTED_EDGE('',*,*,#7730,.T.);
#10074=ORIENTED_EDGE('',*,*,#7731,.T.);
#10075=ORIENTED_EDGE('',*,*,#7730,.F.);
#10076=ORIENTED_EDGE('',*,*,#7729,.T.);
#10077=ORIENTED_EDGE('',*,*,#7726,.T.);
#10078=ORIENTED_EDGE('',*,*,#7731,.F.);
#10079=ORIENTED_EDGE('',*,*,#7728,.F.);
#10080=ORIENTED_EDGE('',*,*,#7732,.F.);
#10081=ORIENTED_EDGE('',*,*,#7733,.T.);
#10082=ORIENTED_EDGE('',*,*,#7734,.F.);
#10083=ORIENTED_EDGE('',*,*,#7733,.F.);
#10084=ORIENTED_EDGE('',*,*,#7732,.T.);
#10085=ORIENTED_EDGE('',*,*,#7735,.F.);
#10086=ORIENTED_EDGE('',*,*,#7736,.F.);
#10087=ORIENTED_EDGE('',*,*,#7737,.T.);
#10088=ORIENTED_EDGE('',*,*,#7735,.T.);
#10089=ORIENTED_EDGE('',*,*,#7737,.F.);
#10090=ORIENTED_EDGE('',*,*,#7738,.F.);
#10091=ORIENTED_EDGE('',*,*,#7739,.T.);
#10092=ORIENTED_EDGE('',*,*,#7740,.F.);
#10093=ORIENTED_EDGE('',*,*,#7739,.F.);
#10094=ORIENTED_EDGE('',*,*,#7738,.T.);
#10095=ORIENTED_EDGE('',*,*,#7741,.F.);
#10096=ORIENTED_EDGE('',*,*,#7742,.F.);
#10097=ORIENTED_EDGE('',*,*,#7743,.T.);
#10098=ORIENTED_EDGE('',*,*,#7741,.T.);
#10099=ORIENTED_EDGE('',*,*,#7743,.F.);
#10100=ORIENTED_EDGE('',*,*,#7744,.T.);
#10101=ORIENTED_EDGE('',*,*,#7745,.T.);
#10102=ORIENTED_EDGE('',*,*,#7746,.F.);
#10103=ORIENTED_EDGE('',*,*,#7747,.F.);
#10104=ORIENTED_EDGE('',*,*,#7748,.T.);
#10105=ORIENTED_EDGE('',*,*,#7747,.T.);
#10106=ORIENTED_EDGE('',*,*,#7749,.F.);
#10107=ORIENTED_EDGE('',*,*,#7750,.F.);
#10108=ORIENTED_EDGE('',*,*,#7751,.T.);
#10109=ORIENTED_EDGE('',*,*,#7750,.T.);
#10110=ORIENTED_EDGE('',*,*,#7752,.F.);
#10111=ORIENTED_EDGE('',*,*,#7753,.F.);
#10112=ORIENTED_EDGE('',*,*,#7754,.T.);
#10113=ORIENTED_EDGE('',*,*,#7753,.T.);
#10114=ORIENTED_EDGE('',*,*,#7755,.F.);
#10115=ORIENTED_EDGE('',*,*,#7745,.F.);
#10116=ORIENTED_EDGE('',*,*,#7755,.T.);
#10117=ORIENTED_EDGE('',*,*,#7752,.T.);
#10118=ORIENTED_EDGE('',*,*,#7749,.T.);
#10119=ORIENTED_EDGE('',*,*,#7746,.T.);
#10120=ORIENTED_EDGE('',*,*,#7734,.T.);
#10121=ORIENTED_EDGE('',*,*,#7740,.T.);
#10122=ORIENTED_EDGE('',*,*,#7754,.F.);
#10123=ORIENTED_EDGE('',*,*,#7744,.F.);
#10124=ORIENTED_EDGE('',*,*,#7748,.F.);
#10125=ORIENTED_EDGE('',*,*,#7751,.F.);
#10126=ORIENTED_EDGE('',*,*,#7736,.T.);
#10127=ORIENTED_EDGE('',*,*,#7742,.T.);
#10128=ORIENTED_EDGE('',*,*,#7756,.T.);
#10129=ORIENTED_EDGE('',*,*,#7757,.T.);
#10130=ORIENTED_EDGE('',*,*,#7758,.F.);
#10131=ORIENTED_EDGE('',*,*,#7759,.F.);
#10132=ORIENTED_EDGE('',*,*,#7760,.T.);
#10133=ORIENTED_EDGE('',*,*,#7759,.T.);
#10134=ORIENTED_EDGE('',*,*,#7761,.F.);
#10135=ORIENTED_EDGE('',*,*,#7762,.F.);
#10136=ORIENTED_EDGE('',*,*,#7763,.T.);
#10137=ORIENTED_EDGE('',*,*,#7762,.T.);
#10138=ORIENTED_EDGE('',*,*,#7764,.F.);
#10139=ORIENTED_EDGE('',*,*,#7765,.F.);
#10140=ORIENTED_EDGE('',*,*,#7766,.T.);
#10141=ORIENTED_EDGE('',*,*,#7765,.T.);
#10142=ORIENTED_EDGE('',*,*,#7767,.F.);
#10143=ORIENTED_EDGE('',*,*,#7757,.F.);
#10144=ORIENTED_EDGE('',*,*,#7767,.T.);
#10145=ORIENTED_EDGE('',*,*,#7764,.T.);
#10146=ORIENTED_EDGE('',*,*,#7761,.T.);
#10147=ORIENTED_EDGE('',*,*,#7758,.T.);
#10148=ORIENTED_EDGE('',*,*,#7766,.F.);
#10149=ORIENTED_EDGE('',*,*,#7756,.F.);
#10150=ORIENTED_EDGE('',*,*,#7760,.F.);
#10151=ORIENTED_EDGE('',*,*,#7763,.F.);
#10152=ORIENTED_EDGE('',*,*,#7768,.F.);
#10153=ORIENTED_EDGE('',*,*,#7769,.T.);
#10154=ORIENTED_EDGE('',*,*,#7770,.F.);
#10155=ORIENTED_EDGE('',*,*,#7769,.F.);
#10156=ORIENTED_EDGE('',*,*,#7771,.F.);
#10157=ORIENTED_EDGE('',*,*,#7772,.T.);
#10158=ORIENTED_EDGE('',*,*,#7773,.F.);
#10159=ORIENTED_EDGE('',*,*,#7772,.F.);
#10160=ORIENTED_EDGE('',*,*,#7774,.T.);
#10161=ORIENTED_EDGE('',*,*,#7775,.T.);
#10162=ORIENTED_EDGE('',*,*,#7776,.F.);
#10163=ORIENTED_EDGE('',*,*,#7777,.F.);
#10164=ORIENTED_EDGE('',*,*,#7770,.T.);
#10165=ORIENTED_EDGE('',*,*,#7773,.T.);
#10166=ORIENTED_EDGE('',*,*,#7778,.T.);
#10167=ORIENTED_EDGE('',*,*,#7777,.T.);
#10168=ORIENTED_EDGE('',*,*,#7779,.F.);
#10169=ORIENTED_EDGE('',*,*,#7780,.F.);
#10170=ORIENTED_EDGE('',*,*,#7781,.T.);
#10171=ORIENTED_EDGE('',*,*,#7780,.T.);
#10172=ORIENTED_EDGE('',*,*,#7782,.F.);
#10173=ORIENTED_EDGE('',*,*,#7783,.F.);
#10174=ORIENTED_EDGE('',*,*,#7768,.T.);
#10175=ORIENTED_EDGE('',*,*,#7771,.T.);
#10176=ORIENTED_EDGE('',*,*,#7784,.T.);
#10177=ORIENTED_EDGE('',*,*,#7783,.T.);
#10178=ORIENTED_EDGE('',*,*,#7785,.F.);
#10179=ORIENTED_EDGE('',*,*,#7775,.F.);
#10180=ORIENTED_EDGE('',*,*,#7785,.T.);
#10181=ORIENTED_EDGE('',*,*,#7782,.T.);
#10182=ORIENTED_EDGE('',*,*,#7779,.T.);
#10183=ORIENTED_EDGE('',*,*,#7776,.T.);
#10184=ORIENTED_EDGE('',*,*,#7784,.F.);
#10185=ORIENTED_EDGE('',*,*,#7774,.F.);
#10186=ORIENTED_EDGE('',*,*,#7778,.F.);
#10187=ORIENTED_EDGE('',*,*,#7781,.F.);
#10188=ORIENTED_EDGE('',*,*,#7786,.F.);
#10189=ORIENTED_EDGE('',*,*,#7787,.T.);
#10190=ORIENTED_EDGE('',*,*,#7788,.F.);
#10191=ORIENTED_EDGE('',*,*,#7787,.F.);
#10192=ORIENTED_EDGE('',*,*,#7789,.F.);
#10193=ORIENTED_EDGE('',*,*,#7790,.T.);
#10194=ORIENTED_EDGE('',*,*,#7791,.F.);
#10195=ORIENTED_EDGE('',*,*,#7790,.F.);
#10196=ORIENTED_EDGE('',*,*,#7792,.T.);
#10197=ORIENTED_EDGE('',*,*,#7793,.T.);
#10198=ORIENTED_EDGE('',*,*,#7794,.F.);
#10199=ORIENTED_EDGE('',*,*,#7795,.F.);
#10200=ORIENTED_EDGE('',*,*,#7788,.T.);
#10201=ORIENTED_EDGE('',*,*,#7791,.T.);
#10202=ORIENTED_EDGE('',*,*,#7796,.T.);
#10203=ORIENTED_EDGE('',*,*,#7795,.T.);
#10204=ORIENTED_EDGE('',*,*,#7797,.F.);
#10205=ORIENTED_EDGE('',*,*,#7798,.F.);
#10206=ORIENTED_EDGE('',*,*,#7799,.T.);
#10207=ORIENTED_EDGE('',*,*,#7798,.T.);
#10208=ORIENTED_EDGE('',*,*,#7800,.F.);
#10209=ORIENTED_EDGE('',*,*,#7801,.F.);
#10210=ORIENTED_EDGE('',*,*,#7786,.T.);
#10211=ORIENTED_EDGE('',*,*,#7789,.T.);
#10212=ORIENTED_EDGE('',*,*,#7802,.T.);
#10213=ORIENTED_EDGE('',*,*,#7801,.T.);
#10214=ORIENTED_EDGE('',*,*,#7803,.F.);
#10215=ORIENTED_EDGE('',*,*,#7793,.F.);
#10216=ORIENTED_EDGE('',*,*,#7803,.T.);
#10217=ORIENTED_EDGE('',*,*,#7800,.T.);
#10218=ORIENTED_EDGE('',*,*,#7797,.T.);
#10219=ORIENTED_EDGE('',*,*,#7794,.T.);
#10220=ORIENTED_EDGE('',*,*,#7802,.F.);
#10221=ORIENTED_EDGE('',*,*,#7792,.F.);
#10222=ORIENTED_EDGE('',*,*,#7796,.F.);
#10223=ORIENTED_EDGE('',*,*,#7799,.F.);
#10224=ORIENTED_EDGE('',*,*,#7804,.F.);
#10225=ORIENTED_EDGE('',*,*,#7805,.T.);
#10226=ORIENTED_EDGE('',*,*,#7806,.F.);
#10227=ORIENTED_EDGE('',*,*,#7805,.F.);
#10228=ORIENTED_EDGE('',*,*,#7807,.F.);
#10229=ORIENTED_EDGE('',*,*,#7808,.T.);
#10230=ORIENTED_EDGE('',*,*,#7809,.F.);
#10231=ORIENTED_EDGE('',*,*,#7808,.F.);
#10232=ORIENTED_EDGE('',*,*,#7810,.F.);
#10233=ORIENTED_EDGE('',*,*,#7811,.T.);
#10234=ORIENTED_EDGE('',*,*,#7812,.F.);
#10235=ORIENTED_EDGE('',*,*,#7811,.F.);
#10236=ORIENTED_EDGE('',*,*,#7813,.F.);
#10237=ORIENTED_EDGE('',*,*,#7814,.T.);
#10238=ORIENTED_EDGE('',*,*,#7815,.F.);
#10239=ORIENTED_EDGE('',*,*,#7814,.F.);
#10240=ORIENTED_EDGE('',*,*,#7816,.F.);
#10241=ORIENTED_EDGE('',*,*,#7817,.T.);
#10242=ORIENTED_EDGE('',*,*,#7818,.F.);
#10243=ORIENTED_EDGE('',*,*,#7819,.F.);
#10244=ORIENTED_EDGE('',*,*,#7820,.F.);
#10245=ORIENTED_EDGE('',*,*,#7819,.T.);
#10246=ORIENTED_EDGE('',*,*,#7821,.F.);
#10247=ORIENTED_EDGE('',*,*,#7822,.F.);
#10248=ORIENTED_EDGE('',*,*,#7823,.F.);
#10249=ORIENTED_EDGE('',*,*,#7822,.T.);
#10250=ORIENTED_EDGE('',*,*,#7824,.F.);
#10251=ORIENTED_EDGE('',*,*,#7825,.F.);
#10252=ORIENTED_EDGE('',*,*,#7826,.F.);
#10253=ORIENTED_EDGE('',*,*,#7825,.T.);
#10254=ORIENTED_EDGE('',*,*,#7827,.F.);
#10255=ORIENTED_EDGE('',*,*,#7817,.F.);
#10256=ORIENTED_EDGE('',*,*,#7827,.T.);
#10257=ORIENTED_EDGE('',*,*,#7824,.T.);
#10258=ORIENTED_EDGE('',*,*,#7821,.T.);
#10259=ORIENTED_EDGE('',*,*,#7818,.T.);
#10260=ORIENTED_EDGE('',*,*,#7806,.T.);
#10261=ORIENTED_EDGE('',*,*,#7809,.T.);
#10262=ORIENTED_EDGE('',*,*,#7812,.T.);
#10263=ORIENTED_EDGE('',*,*,#7815,.T.);
#10264=ORIENTED_EDGE('',*,*,#7826,.T.);
#10265=ORIENTED_EDGE('',*,*,#7816,.T.);
#10266=ORIENTED_EDGE('',*,*,#7820,.T.);
#10267=ORIENTED_EDGE('',*,*,#7823,.T.);
#10268=ORIENTED_EDGE('',*,*,#7804,.T.);
#10269=ORIENTED_EDGE('',*,*,#7807,.T.);
#10270=ORIENTED_EDGE('',*,*,#7810,.T.);
#10271=ORIENTED_EDGE('',*,*,#7813,.T.);
#10272=ORIENTED_EDGE('',*,*,#7828,.F.);
#10273=ORIENTED_EDGE('',*,*,#7829,.F.);
#10274=ORIENTED_EDGE('',*,*,#7830,.T.);
#10275=ORIENTED_EDGE('',*,*,#7831,.F.);
#10276=ORIENTED_EDGE('',*,*,#7832,.F.);
#10277=ORIENTED_EDGE('',*,*,#7830,.F.);
#10278=ORIENTED_EDGE('',*,*,#7831,.T.);
#10279=ORIENTED_EDGE('',*,*,#7832,.T.);
#10280=ORIENTED_EDGE('',*,*,#7833,.T.);
#10281=ORIENTED_EDGE('',*,*,#7834,.T.);
#10282=ORIENTED_EDGE('',*,*,#7833,.F.);
#10283=ORIENTED_EDGE('',*,*,#7835,.T.);
#10284=ORIENTED_EDGE('',*,*,#7836,.T.);
#10285=ORIENTED_EDGE('',*,*,#7837,.F.);
#10286=ORIENTED_EDGE('',*,*,#7836,.F.);
#10287=ORIENTED_EDGE('',*,*,#7837,.T.);
#10288=ORIENTED_EDGE('',*,*,#7838,.T.);
#10289=ORIENTED_EDGE('',*,*,#7839,.F.);
#10290=ORIENTED_EDGE('',*,*,#7838,.F.);
#10291=ORIENTED_EDGE('',*,*,#7834,.F.);
#10292=ORIENTED_EDGE('',*,*,#7839,.T.);
#10293=ORIENTED_EDGE('',*,*,#7840,.F.);
#10294=ORIENTED_EDGE('',*,*,#7841,.T.);
#10295=ORIENTED_EDGE('',*,*,#7828,.T.);
#10296=ORIENTED_EDGE('',*,*,#7829,.T.);
#10297=ORIENTED_EDGE('',*,*,#7841,.F.);
#10298=ORIENTED_EDGE('',*,*,#7840,.T.);
#10299=ORIENTED_EDGE('',*,*,#7842,.F.);
#10300=ORIENTED_EDGE('',*,*,#7842,.T.);
#10301=ORIENTED_EDGE('',*,*,#7843,.T.);
#10302=ORIENTED_EDGE('',*,*,#7835,.F.);
#10303=ORIENTED_EDGE('',*,*,#7843,.F.);
#10304=ORIENTED_EDGE('',*,*,#7844,.F.);
#10305=ORIENTED_EDGE('',*,*,#7845,.F.);
#10306=ORIENTED_EDGE('',*,*,#7846,.T.);
#10307=ORIENTED_EDGE('',*,*,#7847,.F.);
#10308=ORIENTED_EDGE('',*,*,#7848,.F.);
#10309=ORIENTED_EDGE('',*,*,#7846,.F.);
#10310=ORIENTED_EDGE('',*,*,#7849,.T.);
#10311=ORIENTED_EDGE('',*,*,#7850,.T.);
#10312=ORIENTED_EDGE('',*,*,#7847,.T.);
#10313=ORIENTED_EDGE('',*,*,#7848,.T.);
#10314=ORIENTED_EDGE('',*,*,#7850,.F.);
#10315=ORIENTED_EDGE('',*,*,#7851,.F.);
#10316=ORIENTED_EDGE('',*,*,#7852,.T.);
#10317=ORIENTED_EDGE('',*,*,#7853,.F.);
#10318=ORIENTED_EDGE('',*,*,#7854,.T.);
#10319=ORIENTED_EDGE('',*,*,#7851,.T.);
#10320=ORIENTED_EDGE('',*,*,#7854,.F.);
#10321=ORIENTED_EDGE('',*,*,#7855,.F.);
#10322=ORIENTED_EDGE('',*,*,#7856,.T.);
#10323=ORIENTED_EDGE('',*,*,#7853,.T.);
#10324=ORIENTED_EDGE('',*,*,#7856,.F.);
#10325=ORIENTED_EDGE('',*,*,#7857,.F.);
#10326=ORIENTED_EDGE('',*,*,#7858,.T.);
#10327=ORIENTED_EDGE('',*,*,#7855,.T.);
#10328=ORIENTED_EDGE('',*,*,#7858,.F.);
#10329=ORIENTED_EDGE('',*,*,#7857,.T.);
#10330=ORIENTED_EDGE('',*,*,#7849,.F.);
#10331=ORIENTED_EDGE('',*,*,#7844,.T.);
#10332=ORIENTED_EDGE('',*,*,#7845,.T.);
#10333=ORIENTED_EDGE('',*,*,#7859,.T.);
#10334=ORIENTED_EDGE('',*,*,#7852,.F.);
#10335=ORIENTED_EDGE('',*,*,#7859,.F.);
#10336=ORIENTED_EDGE('',*,*,#7860,.T.);
#10337=ORIENTED_EDGE('',*,*,#7860,.F.);
#10338=ORIENTED_EDGE('',*,*,#7861,.T.);
#10339=ORIENTED_EDGE('',*,*,#7861,.F.);
#10340=ORIENTED_EDGE('',*,*,#7862,.T.);
#10341=ORIENTED_EDGE('',*,*,#7862,.F.);
#10342=ORIENTED_EDGE('',*,*,#7863,.T.);
#10343=ORIENTED_EDGE('',*,*,#7863,.F.);
#10344=ORIENTED_EDGE('',*,*,#7864,.T.);
#10345=ORIENTED_EDGE('',*,*,#7864,.F.);
#10346=ORIENTED_EDGE('',*,*,#7865,.T.);
#10347=ORIENTED_EDGE('',*,*,#7865,.F.);
#10348=ORIENTED_EDGE('',*,*,#7866,.T.);
#10349=ORIENTED_EDGE('',*,*,#7866,.F.);
#10350=ORIENTED_EDGE('',*,*,#7867,.T.);
#10351=ORIENTED_EDGE('',*,*,#7867,.F.);
#10352=ORIENTED_EDGE('',*,*,#7868,.F.);
#10353=ORIENTED_EDGE('',*,*,#7869,.F.);
#10354=ORIENTED_EDGE('',*,*,#7870,.F.);
#10355=ORIENTED_EDGE('',*,*,#7871,.F.);
#10356=ORIENTED_EDGE('',*,*,#7870,.T.);
#10357=ORIENTED_EDGE('',*,*,#7872,.F.);
#10358=ORIENTED_EDGE('',*,*,#7873,.T.);
#10359=ORIENTED_EDGE('',*,*,#7874,.F.);
#10360=ORIENTED_EDGE('',*,*,#7875,.T.);
#10361=ORIENTED_EDGE('',*,*,#7876,.F.);
#10362=ORIENTED_EDGE('',*,*,#7877,.T.);
#10363=ORIENTED_EDGE('',*,*,#7878,.T.);
#10364=ORIENTED_EDGE('',*,*,#7879,.F.);
#10365=ORIENTED_EDGE('',*,*,#7878,.F.);
#10366=ORIENTED_EDGE('',*,*,#7880,.T.);
#10367=ORIENTED_EDGE('',*,*,#7881,.F.);
#10368=ORIENTED_EDGE('',*,*,#7882,.T.);
#10369=ORIENTED_EDGE('',*,*,#7883,.F.);
#10370=ORIENTED_EDGE('',*,*,#7884,.T.);
#10371=ORIENTED_EDGE('',*,*,#7885,.F.);
#10372=ORIENTED_EDGE('',*,*,#7886,.T.);
#10373=ORIENTED_EDGE('',*,*,#7887,.F.);
#10374=ORIENTED_EDGE('',*,*,#7888,.T.);
#10375=ORIENTED_EDGE('',*,*,#7889,.F.);
#10376=ORIENTED_EDGE('',*,*,#7869,.T.);
#10377=ORIENTED_EDGE('',*,*,#7890,.T.);
#10378=ORIENTED_EDGE('',*,*,#7891,.T.);
#10379=ORIENTED_EDGE('',*,*,#7872,.T.);
#10380=ORIENTED_EDGE('',*,*,#7892,.F.);
#10381=ORIENTED_EDGE('',*,*,#7893,.F.);
#10382=ORIENTED_EDGE('',*,*,#7873,.F.);
#10383=ORIENTED_EDGE('',*,*,#7891,.F.);
#10384=ORIENTED_EDGE('',*,*,#7893,.T.);
#10385=ORIENTED_EDGE('',*,*,#7894,.T.);
#10386=ORIENTED_EDGE('',*,*,#7895,.T.);
#10387=ORIENTED_EDGE('',*,*,#7874,.T.);
#10388=ORIENTED_EDGE('',*,*,#7896,.F.);
#10389=ORIENTED_EDGE('',*,*,#7897,.F.);
#10390=ORIENTED_EDGE('',*,*,#7875,.F.);
#10391=ORIENTED_EDGE('',*,*,#7895,.F.);
#10392=ORIENTED_EDGE('',*,*,#7897,.T.);
#10393=ORIENTED_EDGE('',*,*,#7898,.T.);
#10394=ORIENTED_EDGE('',*,*,#7899,.T.);
#10395=ORIENTED_EDGE('',*,*,#7876,.T.);
#10396=ORIENTED_EDGE('',*,*,#7900,.F.);
#10397=ORIENTED_EDGE('',*,*,#7901,.F.);
#10398=ORIENTED_EDGE('',*,*,#7880,.F.);
#10399=ORIENTED_EDGE('',*,*,#7877,.F.);
#10400=ORIENTED_EDGE('',*,*,#7899,.F.);
#10401=ORIENTED_EDGE('',*,*,#7902,.F.);
#10402=ORIENTED_EDGE('',*,*,#7901,.T.);
#10403=ORIENTED_EDGE('',*,*,#7903,.T.);
#10404=ORIENTED_EDGE('',*,*,#7904,.T.);
#10405=ORIENTED_EDGE('',*,*,#7881,.T.);
#10406=ORIENTED_EDGE('',*,*,#7905,.F.);
#10407=ORIENTED_EDGE('',*,*,#7906,.F.);
#10408=ORIENTED_EDGE('',*,*,#7882,.F.);
#10409=ORIENTED_EDGE('',*,*,#7904,.F.);
#10410=ORIENTED_EDGE('',*,*,#7906,.T.);
#10411=ORIENTED_EDGE('',*,*,#7907,.T.);
#10412=ORIENTED_EDGE('',*,*,#7908,.T.);
#10413=ORIENTED_EDGE('',*,*,#7883,.T.);
#10414=ORIENTED_EDGE('',*,*,#7909,.F.);
#10415=ORIENTED_EDGE('',*,*,#7910,.F.);
#10416=ORIENTED_EDGE('',*,*,#7884,.F.);
#10417=ORIENTED_EDGE('',*,*,#7908,.F.);
#10418=ORIENTED_EDGE('',*,*,#7910,.T.);
#10419=ORIENTED_EDGE('',*,*,#7911,.T.);
#10420=ORIENTED_EDGE('',*,*,#7912,.T.);
#10421=ORIENTED_EDGE('',*,*,#7885,.T.);
#10422=ORIENTED_EDGE('',*,*,#7886,.F.);
#10423=ORIENTED_EDGE('',*,*,#7912,.F.);
#10424=ORIENTED_EDGE('',*,*,#7913,.F.);
#10425=ORIENTED_EDGE('',*,*,#7914,.F.);
#10426=ORIENTED_EDGE('',*,*,#7915,.F.);
#10427=ORIENTED_EDGE('',*,*,#7916,.T.);
#10428=ORIENTED_EDGE('',*,*,#7902,.T.);
#10429=ORIENTED_EDGE('',*,*,#7898,.F.);
#10430=ORIENTED_EDGE('',*,*,#7896,.T.);
#10431=ORIENTED_EDGE('',*,*,#7894,.F.);
#10432=ORIENTED_EDGE('',*,*,#7892,.T.);
#10433=ORIENTED_EDGE('',*,*,#7890,.F.);
#10434=ORIENTED_EDGE('',*,*,#7868,.T.);
#10435=ORIENTED_EDGE('',*,*,#7917,.F.);
#10436=ORIENTED_EDGE('',*,*,#7918,.T.);
#10437=ORIENTED_EDGE('',*,*,#7919,.F.);
#10438=ORIENTED_EDGE('',*,*,#7913,.T.);
#10439=ORIENTED_EDGE('',*,*,#7911,.F.);
#10440=ORIENTED_EDGE('',*,*,#7909,.T.);
#10441=ORIENTED_EDGE('',*,*,#7907,.F.);
#10442=ORIENTED_EDGE('',*,*,#7905,.T.);
#10443=ORIENTED_EDGE('',*,*,#7903,.F.);
#10444=ORIENTED_EDGE('',*,*,#7900,.T.);
#10445=ORIENTED_EDGE('',*,*,#7916,.F.);
#10446=ORIENTED_EDGE('',*,*,#7871,.T.);
#10447=ORIENTED_EDGE('',*,*,#7889,.T.);
#10448=ORIENTED_EDGE('',*,*,#7920,.T.);
#10449=ORIENTED_EDGE('',*,*,#7917,.T.);
#10450=ORIENTED_EDGE('',*,*,#7888,.F.);
#10451=ORIENTED_EDGE('',*,*,#7921,.F.);
#10452=ORIENTED_EDGE('',*,*,#7918,.F.);
#10453=ORIENTED_EDGE('',*,*,#7920,.F.);
#10454=ORIENTED_EDGE('',*,*,#7879,.T.);
#10455=ORIENTED_EDGE('',*,*,#7915,.T.);
#10456=ORIENTED_EDGE('',*,*,#7914,.T.);
#10457=ORIENTED_EDGE('',*,*,#7919,.T.);
#10458=ORIENTED_EDGE('',*,*,#7921,.T.);
#10459=ORIENTED_EDGE('',*,*,#7887,.T.);
#10460=ORIENTED_EDGE('',*,*,#7922,.F.);
#10461=ORIENTED_EDGE('',*,*,#7923,.T.);
#10462=ORIENTED_EDGE('',*,*,#7924,.F.);
#10463=ORIENTED_EDGE('',*,*,#7925,.T.);
#10464=ORIENTED_EDGE('',*,*,#7922,.T.);
#10465=ORIENTED_EDGE('',*,*,#7925,.F.);
#10466=ORIENTED_EDGE('',*,*,#7924,.T.);
#10467=ORIENTED_EDGE('',*,*,#7926,.F.);
#10468=ORIENTED_EDGE('',*,*,#7926,.T.);
#10469=ORIENTED_EDGE('',*,*,#7927,.T.);
#10470=ORIENTED_EDGE('',*,*,#7923,.F.);
#10471=ORIENTED_EDGE('',*,*,#7927,.F.);
#10472=ORIENTED_EDGE('',*,*,#7928,.F.);
#10473=ORIENTED_EDGE('',*,*,#7929,.T.);
#10474=ORIENTED_EDGE('',*,*,#7930,.F.);
#10475=ORIENTED_EDGE('',*,*,#7931,.T.);
#10476=ORIENTED_EDGE('',*,*,#7928,.T.);
#10477=ORIENTED_EDGE('',*,*,#7931,.F.);
#10478=ORIENTED_EDGE('',*,*,#7930,.T.);
#10479=ORIENTED_EDGE('',*,*,#7932,.F.);
#10480=ORIENTED_EDGE('',*,*,#7932,.T.);
#10481=ORIENTED_EDGE('',*,*,#7933,.T.);
#10482=ORIENTED_EDGE('',*,*,#7929,.F.);
#10483=ORIENTED_EDGE('',*,*,#7933,.F.);
#10484=ORIENTED_EDGE('',*,*,#7934,.T.);
#10485=ORIENTED_EDGE('',*,*,#7935,.T.);
#10486=ORIENTED_EDGE('',*,*,#7936,.T.);
#10487=ORIENTED_EDGE('',*,*,#7937,.F.);
#10488=ORIENTED_EDGE('',*,*,#7938,.T.);
#10489=ORIENTED_EDGE('',*,*,#7939,.T.);
#10490=ORIENTED_EDGE('',*,*,#7940,.T.);
#10491=ORIENTED_EDGE('',*,*,#7935,.F.);
#10492=ORIENTED_EDGE('',*,*,#7941,.T.);
#10493=ORIENTED_EDGE('',*,*,#7942,.T.);
#10494=ORIENTED_EDGE('',*,*,#7943,.T.);
#10495=ORIENTED_EDGE('',*,*,#7939,.F.);
#10496=ORIENTED_EDGE('',*,*,#7944,.T.);
#10497=ORIENTED_EDGE('',*,*,#7945,.T.);
#10498=ORIENTED_EDGE('',*,*,#7946,.T.);
#10499=ORIENTED_EDGE('',*,*,#7942,.F.);
#10500=ORIENTED_EDGE('',*,*,#7947,.T.);
#10501=ORIENTED_EDGE('',*,*,#7948,.T.);
#10502=ORIENTED_EDGE('',*,*,#7949,.T.);
#10503=ORIENTED_EDGE('',*,*,#7945,.F.);
#10504=ORIENTED_EDGE('',*,*,#7950,.T.);
#10505=ORIENTED_EDGE('',*,*,#7937,.T.);
#10506=ORIENTED_EDGE('',*,*,#7951,.T.);
#10507=ORIENTED_EDGE('',*,*,#7948,.F.);
#10508=ORIENTED_EDGE('',*,*,#7950,.F.);
#10509=ORIENTED_EDGE('',*,*,#7947,.F.);
#10510=ORIENTED_EDGE('',*,*,#7944,.F.);
#10511=ORIENTED_EDGE('',*,*,#7941,.F.);
#10512=ORIENTED_EDGE('',*,*,#7938,.F.);
#10513=ORIENTED_EDGE('',*,*,#7934,.F.);
#10514=ORIENTED_EDGE('',*,*,#7951,.F.);
#10515=ORIENTED_EDGE('',*,*,#7936,.F.);
#10516=ORIENTED_EDGE('',*,*,#7940,.F.);
#10517=ORIENTED_EDGE('',*,*,#7943,.F.);
#10518=ORIENTED_EDGE('',*,*,#7946,.F.);
#10519=ORIENTED_EDGE('',*,*,#7949,.F.);
#10520=ORIENTED_EDGE('',*,*,#7952,.T.);
#10521=ORIENTED_EDGE('',*,*,#7953,.T.);
#10522=ORIENTED_EDGE('',*,*,#7952,.F.);
#10523=ORIENTED_EDGE('',*,*,#7954,.T.);
#10524=ORIENTED_EDGE('',*,*,#7955,.T.);
#10525=ORIENTED_EDGE('',*,*,#7954,.F.);
#10526=ORIENTED_EDGE('',*,*,#7955,.F.);
#10527=ORIENTED_EDGE('',*,*,#7956,.F.);
#10528=ORIENTED_EDGE('',*,*,#7957,.F.);
#10529=ORIENTED_EDGE('',*,*,#7958,.T.);
#10530=ORIENTED_EDGE('',*,*,#7956,.T.);
#10531=ORIENTED_EDGE('',*,*,#7958,.F.);
#10532=ORIENTED_EDGE('',*,*,#7959,.F.);
#10533=ORIENTED_EDGE('',*,*,#7960,.T.);
#10534=ORIENTED_EDGE('',*,*,#7957,.T.);
#10535=ORIENTED_EDGE('',*,*,#7960,.F.);
#10536=ORIENTED_EDGE('',*,*,#7961,.F.);
#10537=ORIENTED_EDGE('',*,*,#7962,.T.);
#10538=ORIENTED_EDGE('',*,*,#7959,.T.);
#10539=ORIENTED_EDGE('',*,*,#7962,.F.);
#10540=ORIENTED_EDGE('',*,*,#7961,.T.);
#10541=ORIENTED_EDGE('',*,*,#7963,.F.);
#10542=ORIENTED_EDGE('',*,*,#7964,.F.);
#10543=ORIENTED_EDGE('',*,*,#7965,.T.);
#10544=ORIENTED_EDGE('',*,*,#7963,.T.);
#10545=ORIENTED_EDGE('',*,*,#7965,.F.);
#10546=ORIENTED_EDGE('',*,*,#7966,.F.);
#10547=ORIENTED_EDGE('',*,*,#7967,.T.);
#10548=ORIENTED_EDGE('',*,*,#7964,.T.);
#10549=ORIENTED_EDGE('',*,*,#7967,.F.);
#10550=ORIENTED_EDGE('',*,*,#7953,.F.);
#10551=ORIENTED_EDGE('',*,*,#7968,.T.);
#10552=ORIENTED_EDGE('',*,*,#7966,.T.);
#10553=ORIENTED_EDGE('',*,*,#7968,.F.);
#10554=ORIENTED_EDGE('',*,*,#7969,.F.);
#10555=ORIENTED_EDGE('',*,*,#7970,.F.);
#10556=ORIENTED_EDGE('',*,*,#7971,.T.);
#10557=ORIENTED_EDGE('',*,*,#7972,.F.);
#10558=ORIENTED_EDGE('',*,*,#7973,.F.);
#10559=ORIENTED_EDGE('',*,*,#7971,.F.);
#10560=ORIENTED_EDGE('',*,*,#7972,.T.);
#10561=ORIENTED_EDGE('',*,*,#7973,.T.);
#10562=ORIENTED_EDGE('',*,*,#7974,.T.);
#10563=ORIENTED_EDGE('',*,*,#7975,.T.);
#10564=ORIENTED_EDGE('',*,*,#7974,.F.);
#10565=ORIENTED_EDGE('',*,*,#7976,.T.);
#10566=ORIENTED_EDGE('',*,*,#7977,.T.);
#10567=ORIENTED_EDGE('',*,*,#7978,.F.);
#10568=ORIENTED_EDGE('',*,*,#7977,.F.);
#10569=ORIENTED_EDGE('',*,*,#7978,.T.);
#10570=ORIENTED_EDGE('',*,*,#7979,.T.);
#10571=ORIENTED_EDGE('',*,*,#7980,.F.);
#10572=ORIENTED_EDGE('',*,*,#7979,.F.);
#10573=ORIENTED_EDGE('',*,*,#7975,.F.);
#10574=ORIENTED_EDGE('',*,*,#7980,.T.);
#10575=ORIENTED_EDGE('',*,*,#7981,.F.);
#10576=ORIENTED_EDGE('',*,*,#7982,.T.);
#10577=ORIENTED_EDGE('',*,*,#7969,.T.);
#10578=ORIENTED_EDGE('',*,*,#7970,.T.);
#10579=ORIENTED_EDGE('',*,*,#7982,.F.);
#10580=ORIENTED_EDGE('',*,*,#7981,.T.);
#10581=ORIENTED_EDGE('',*,*,#7983,.F.);
#10582=ORIENTED_EDGE('',*,*,#7983,.T.);
#10583=ORIENTED_EDGE('',*,*,#7984,.T.);
#10584=ORIENTED_EDGE('',*,*,#7976,.F.);
#10585=ORIENTED_EDGE('',*,*,#7984,.F.);
#10586=ORIENTED_EDGE('',*,*,#7985,.F.);
#10587=ORIENTED_EDGE('',*,*,#7986,.F.);
#10588=ORIENTED_EDGE('',*,*,#7987,.T.);
#10589=ORIENTED_EDGE('',*,*,#7988,.F.);
#10590=ORIENTED_EDGE('',*,*,#7989,.F.);
#10591=ORIENTED_EDGE('',*,*,#7987,.F.);
#10592=ORIENTED_EDGE('',*,*,#7990,.T.);
#10593=ORIENTED_EDGE('',*,*,#7991,.T.);
#10594=ORIENTED_EDGE('',*,*,#7988,.T.);
#10595=ORIENTED_EDGE('',*,*,#7989,.T.);
#10596=ORIENTED_EDGE('',*,*,#7991,.F.);
#10597=ORIENTED_EDGE('',*,*,#7992,.F.);
#10598=ORIENTED_EDGE('',*,*,#7993,.T.);
#10599=ORIENTED_EDGE('',*,*,#7994,.F.);
#10600=ORIENTED_EDGE('',*,*,#7995,.T.);
#10601=ORIENTED_EDGE('',*,*,#7992,.T.);
#10602=ORIENTED_EDGE('',*,*,#7995,.F.);
#10603=ORIENTED_EDGE('',*,*,#7996,.F.);
#10604=ORIENTED_EDGE('',*,*,#7997,.T.);
#10605=ORIENTED_EDGE('',*,*,#7994,.T.);
#10606=ORIENTED_EDGE('',*,*,#7997,.F.);
#10607=ORIENTED_EDGE('',*,*,#7998,.F.);
#10608=ORIENTED_EDGE('',*,*,#7999,.T.);
#10609=ORIENTED_EDGE('',*,*,#7996,.T.);
#10610=ORIENTED_EDGE('',*,*,#7999,.F.);
#10611=ORIENTED_EDGE('',*,*,#7998,.T.);
#10612=ORIENTED_EDGE('',*,*,#7990,.F.);
#10613=ORIENTED_EDGE('',*,*,#7985,.T.);
#10614=ORIENTED_EDGE('',*,*,#7986,.T.);
#10615=ORIENTED_EDGE('',*,*,#8000,.T.);
#10616=ORIENTED_EDGE('',*,*,#7993,.F.);
#10617=ORIENTED_EDGE('',*,*,#8000,.F.);
#10618=ORIENTED_EDGE('',*,*,#8001,.T.);
#10619=ORIENTED_EDGE('',*,*,#8001,.F.);
#10620=ORIENTED_EDGE('',*,*,#8002,.T.);
#10621=ORIENTED_EDGE('',*,*,#8002,.F.);
#10622=ORIENTED_EDGE('',*,*,#8003,.T.);
#10623=ORIENTED_EDGE('',*,*,#8003,.F.);
#10624=ORIENTED_EDGE('',*,*,#8004,.T.);
#10625=ORIENTED_EDGE('',*,*,#8004,.F.);
#10626=ORIENTED_EDGE('',*,*,#8005,.T.);
#10627=ORIENTED_EDGE('',*,*,#8005,.F.);
#10628=ORIENTED_EDGE('',*,*,#8006,.T.);
#10629=ORIENTED_EDGE('',*,*,#8006,.F.);
#10630=ORIENTED_EDGE('',*,*,#8007,.T.);
#10631=ORIENTED_EDGE('',*,*,#8007,.F.);
#10632=ORIENTED_EDGE('',*,*,#8008,.F.);
#10633=ORIENTED_EDGE('',*,*,#8009,.F.);
#10634=ORIENTED_EDGE('',*,*,#8010,.F.);
#10635=ORIENTED_EDGE('',*,*,#8011,.F.);
#10636=ORIENTED_EDGE('',*,*,#8010,.T.);
#10637=ORIENTED_EDGE('',*,*,#8012,.F.);
#10638=ORIENTED_EDGE('',*,*,#8013,.T.);
#10639=ORIENTED_EDGE('',*,*,#8014,.F.);
#10640=ORIENTED_EDGE('',*,*,#8015,.T.);
#10641=ORIENTED_EDGE('',*,*,#8016,.F.);
#10642=ORIENTED_EDGE('',*,*,#8017,.T.);
#10643=ORIENTED_EDGE('',*,*,#8018,.F.);
#10644=ORIENTED_EDGE('',*,*,#8017,.F.);
#10645=ORIENTED_EDGE('',*,*,#8019,.F.);
#10646=ORIENTED_EDGE('',*,*,#8020,.T.);
#10647=ORIENTED_EDGE('',*,*,#8021,.F.);
#10648=ORIENTED_EDGE('',*,*,#8022,.T.);
#10649=ORIENTED_EDGE('',*,*,#8023,.F.);
#10650=ORIENTED_EDGE('',*,*,#8024,.T.);
#10651=ORIENTED_EDGE('',*,*,#8025,.F.);
#10652=ORIENTED_EDGE('',*,*,#8026,.T.);
#10653=ORIENTED_EDGE('',*,*,#8027,.F.);
#10654=ORIENTED_EDGE('',*,*,#8009,.T.);
#10655=ORIENTED_EDGE('',*,*,#8028,.T.);
#10656=ORIENTED_EDGE('',*,*,#8029,.T.);
#10657=ORIENTED_EDGE('',*,*,#8012,.T.);
#10658=ORIENTED_EDGE('',*,*,#8030,.F.);
#10659=ORIENTED_EDGE('',*,*,#8031,.F.);
#10660=ORIENTED_EDGE('',*,*,#8013,.F.);
#10661=ORIENTED_EDGE('',*,*,#8029,.F.);
#10662=ORIENTED_EDGE('',*,*,#8031,.T.);
#10663=ORIENTED_EDGE('',*,*,#8032,.T.);
#10664=ORIENTED_EDGE('',*,*,#8033,.T.);
#10665=ORIENTED_EDGE('',*,*,#8014,.T.);
#10666=ORIENTED_EDGE('',*,*,#8034,.F.);
#10667=ORIENTED_EDGE('',*,*,#8035,.F.);
#10668=ORIENTED_EDGE('',*,*,#8015,.F.);
#10669=ORIENTED_EDGE('',*,*,#8033,.F.);
#10670=ORIENTED_EDGE('',*,*,#8035,.T.);
#10671=ORIENTED_EDGE('',*,*,#8036,.T.);
#10672=ORIENTED_EDGE('',*,*,#8037,.T.);
#10673=ORIENTED_EDGE('',*,*,#8038,.T.);
#10674=ORIENTED_EDGE('',*,*,#8019,.T.);
#10675=ORIENTED_EDGE('',*,*,#8016,.T.);
#10676=ORIENTED_EDGE('',*,*,#8039,.F.);
#10677=ORIENTED_EDGE('',*,*,#8040,.F.);
#10678=ORIENTED_EDGE('',*,*,#8020,.F.);
#10679=ORIENTED_EDGE('',*,*,#8038,.F.);
#10680=ORIENTED_EDGE('',*,*,#8040,.T.);
#10681=ORIENTED_EDGE('',*,*,#8041,.T.);
#10682=ORIENTED_EDGE('',*,*,#8042,.T.);
#10683=ORIENTED_EDGE('',*,*,#8021,.T.);
#10684=ORIENTED_EDGE('',*,*,#8043,.F.);
#10685=ORIENTED_EDGE('',*,*,#8044,.F.);
#10686=ORIENTED_EDGE('',*,*,#8022,.F.);
#10687=ORIENTED_EDGE('',*,*,#8042,.F.);
#10688=ORIENTED_EDGE('',*,*,#8044,.T.);
#10689=ORIENTED_EDGE('',*,*,#8045,.T.);
#10690=ORIENTED_EDGE('',*,*,#8046,.T.);
#10691=ORIENTED_EDGE('',*,*,#8023,.T.);
#10692=ORIENTED_EDGE('',*,*,#8024,.F.);
#10693=ORIENTED_EDGE('',*,*,#8046,.F.);
#10694=ORIENTED_EDGE('',*,*,#8047,.F.);
#10695=ORIENTED_EDGE('',*,*,#8048,.F.);
#10696=ORIENTED_EDGE('',*,*,#8049,.F.);
#10697=ORIENTED_EDGE('',*,*,#8050,.T.);
#10698=ORIENTED_EDGE('',*,*,#8036,.F.);
#10699=ORIENTED_EDGE('',*,*,#8034,.T.);
#10700=ORIENTED_EDGE('',*,*,#8032,.F.);
#10701=ORIENTED_EDGE('',*,*,#8030,.T.);
#10702=ORIENTED_EDGE('',*,*,#8028,.F.);
#10703=ORIENTED_EDGE('',*,*,#8008,.T.);
#10704=ORIENTED_EDGE('',*,*,#8051,.F.);
#10705=ORIENTED_EDGE('',*,*,#8052,.T.);
#10706=ORIENTED_EDGE('',*,*,#8053,.F.);
#10707=ORIENTED_EDGE('',*,*,#8047,.T.);
#10708=ORIENTED_EDGE('',*,*,#8045,.F.);
#10709=ORIENTED_EDGE('',*,*,#8043,.T.);
#10710=ORIENTED_EDGE('',*,*,#8041,.F.);
#10711=ORIENTED_EDGE('',*,*,#8039,.T.);
#10712=ORIENTED_EDGE('',*,*,#8037,.F.);
#10713=ORIENTED_EDGE('',*,*,#8050,.F.);
#10714=ORIENTED_EDGE('',*,*,#8011,.T.);
#10715=ORIENTED_EDGE('',*,*,#8027,.T.);
#10716=ORIENTED_EDGE('',*,*,#8054,.T.);
#10717=ORIENTED_EDGE('',*,*,#8051,.T.);
#10718=ORIENTED_EDGE('',*,*,#8026,.F.);
#10719=ORIENTED_EDGE('',*,*,#8055,.F.);
#10720=ORIENTED_EDGE('',*,*,#8052,.F.);
#10721=ORIENTED_EDGE('',*,*,#8054,.F.);
#10722=ORIENTED_EDGE('',*,*,#8018,.T.);
#10723=ORIENTED_EDGE('',*,*,#8049,.T.);
#10724=ORIENTED_EDGE('',*,*,#8048,.T.);
#10725=ORIENTED_EDGE('',*,*,#8053,.T.);
#10726=ORIENTED_EDGE('',*,*,#8055,.T.);
#10727=ORIENTED_EDGE('',*,*,#8025,.T.);
#10728=ORIENTED_EDGE('',*,*,#8056,.F.);
#10729=ORIENTED_EDGE('',*,*,#8057,.T.);
#10730=ORIENTED_EDGE('',*,*,#8058,.F.);
#10731=ORIENTED_EDGE('',*,*,#8059,.T.);
#10732=ORIENTED_EDGE('',*,*,#8056,.T.);
#10733=ORIENTED_EDGE('',*,*,#8059,.F.);
#10734=ORIENTED_EDGE('',*,*,#8058,.T.);
#10735=ORIENTED_EDGE('',*,*,#8060,.F.);
#10736=ORIENTED_EDGE('',*,*,#8060,.T.);
#10737=ORIENTED_EDGE('',*,*,#8061,.T.);
#10738=ORIENTED_EDGE('',*,*,#8057,.F.);
#10739=ORIENTED_EDGE('',*,*,#8061,.F.);
#10740=ORIENTED_EDGE('',*,*,#8062,.F.);
#10741=ORIENTED_EDGE('',*,*,#8063,.T.);
#10742=ORIENTED_EDGE('',*,*,#8064,.F.);
#10743=ORIENTED_EDGE('',*,*,#8065,.T.);
#10744=ORIENTED_EDGE('',*,*,#8062,.T.);
#10745=ORIENTED_EDGE('',*,*,#8065,.F.);
#10746=ORIENTED_EDGE('',*,*,#8064,.T.);
#10747=ORIENTED_EDGE('',*,*,#8066,.F.);
#10748=ORIENTED_EDGE('',*,*,#8066,.T.);
#10749=ORIENTED_EDGE('',*,*,#8067,.T.);
#10750=ORIENTED_EDGE('',*,*,#8063,.F.);
#10751=ORIENTED_EDGE('',*,*,#8067,.F.);
#10752=ORIENTED_EDGE('',*,*,#8068,.F.);
#10753=ORIENTED_EDGE('',*,*,#8069,.F.);
#10754=ORIENTED_EDGE('',*,*,#8070,.T.);
#10755=ORIENTED_EDGE('',*,*,#8068,.T.);
#10756=ORIENTED_EDGE('',*,*,#8070,.F.);
#10757=ORIENTED_EDGE('',*,*,#8071,.F.);
#10758=ORIENTED_EDGE('',*,*,#8072,.T.);
#10759=ORIENTED_EDGE('',*,*,#8069,.T.);
#10760=ORIENTED_EDGE('',*,*,#8072,.F.);
#10761=ORIENTED_EDGE('',*,*,#8073,.F.);
#10762=ORIENTED_EDGE('',*,*,#8074,.T.);
#10763=ORIENTED_EDGE('',*,*,#8071,.T.);
#10764=ORIENTED_EDGE('',*,*,#8074,.F.);
#10765=ORIENTED_EDGE('',*,*,#8073,.T.);
#10766=ORIENTED_EDGE('',*,*,#8075,.F.);
#10767=ORIENTED_EDGE('',*,*,#8076,.F.);
#10768=ORIENTED_EDGE('',*,*,#8077,.T.);
#10769=ORIENTED_EDGE('',*,*,#8075,.T.);
#10770=ORIENTED_EDGE('',*,*,#8077,.F.);
#10771=ORIENTED_EDGE('',*,*,#8078,.F.);
#10772=ORIENTED_EDGE('',*,*,#8079,.T.);
#10773=ORIENTED_EDGE('',*,*,#8076,.T.);
#10774=ORIENTED_EDGE('',*,*,#8079,.F.);
#10775=ORIENTED_EDGE('',*,*,#8080,.F.);
#10776=ORIENTED_EDGE('',*,*,#8081,.T.);
#10777=ORIENTED_EDGE('',*,*,#8078,.T.);
#10778=ORIENTED_EDGE('',*,*,#8081,.F.);
#10779=ORIENTED_EDGE('',*,*,#8080,.T.);
#10780=ORIENTED_EDGE('',*,*,#8082,.T.);
#10781=ORIENTED_EDGE('',*,*,#8083,.T.);
#10782=ORIENTED_EDGE('',*,*,#8084,.T.);
#10783=ORIENTED_EDGE('',*,*,#8085,.F.);
#10784=ORIENTED_EDGE('',*,*,#8086,.T.);
#10785=ORIENTED_EDGE('',*,*,#8087,.T.);
#10786=ORIENTED_EDGE('',*,*,#8088,.T.);
#10787=ORIENTED_EDGE('',*,*,#8083,.F.);
#10788=ORIENTED_EDGE('',*,*,#8089,.T.);
#10789=ORIENTED_EDGE('',*,*,#8090,.T.);
#10790=ORIENTED_EDGE('',*,*,#8091,.T.);
#10791=ORIENTED_EDGE('',*,*,#8087,.F.);
#10792=ORIENTED_EDGE('',*,*,#8092,.T.);
#10793=ORIENTED_EDGE('',*,*,#8093,.T.);
#10794=ORIENTED_EDGE('',*,*,#8094,.T.);
#10795=ORIENTED_EDGE('',*,*,#8090,.F.);
#10796=ORIENTED_EDGE('',*,*,#8095,.T.);
#10797=ORIENTED_EDGE('',*,*,#8096,.T.);
#10798=ORIENTED_EDGE('',*,*,#8097,.T.);
#10799=ORIENTED_EDGE('',*,*,#8093,.F.);
#10800=ORIENTED_EDGE('',*,*,#8098,.T.);
#10801=ORIENTED_EDGE('',*,*,#8085,.T.);
#10802=ORIENTED_EDGE('',*,*,#8099,.T.);
#10803=ORIENTED_EDGE('',*,*,#8096,.F.);
#10804=ORIENTED_EDGE('',*,*,#8098,.F.);
#10805=ORIENTED_EDGE('',*,*,#8095,.F.);
#10806=ORIENTED_EDGE('',*,*,#8092,.F.);
#10807=ORIENTED_EDGE('',*,*,#8089,.F.);
#10808=ORIENTED_EDGE('',*,*,#8086,.F.);
#10809=ORIENTED_EDGE('',*,*,#8082,.F.);
#10810=ORIENTED_EDGE('',*,*,#8099,.F.);
#10811=ORIENTED_EDGE('',*,*,#8084,.F.);
#10812=ORIENTED_EDGE('',*,*,#8088,.F.);
#10813=ORIENTED_EDGE('',*,*,#8091,.F.);
#10814=ORIENTED_EDGE('',*,*,#8094,.F.);
#10815=ORIENTED_EDGE('',*,*,#8097,.F.);
#10816=ORIENTED_EDGE('',*,*,#8100,.F.);
#10817=ORIENTED_EDGE('',*,*,#8101,.T.);
#10818=ORIENTED_EDGE('',*,*,#8102,.F.);
#10819=ORIENTED_EDGE('',*,*,#8101,.F.);
#10820=ORIENTED_EDGE('',*,*,#8103,.F.);
#10821=ORIENTED_EDGE('',*,*,#8104,.T.);
#10822=ORIENTED_EDGE('',*,*,#8105,.F.);
#10823=ORIENTED_EDGE('',*,*,#8104,.F.);
#10824=ORIENTED_EDGE('',*,*,#8106,.T.);
#10825=ORIENTED_EDGE('',*,*,#8106,.F.);
#10826=ORIENTED_EDGE('',*,*,#8103,.T.);
#10827=ORIENTED_EDGE('',*,*,#8102,.T.);
#10828=ORIENTED_EDGE('',*,*,#8107,.F.);
#10829=ORIENTED_EDGE('',*,*,#8108,.T.);
#10830=ORIENTED_EDGE('',*,*,#8109,.F.);
#10831=ORIENTED_EDGE('',*,*,#8110,.F.);
#10832=ORIENTED_EDGE('',*,*,#8111,.F.);
#10833=ORIENTED_EDGE('',*,*,#8112,.T.);
#10834=ORIENTED_EDGE('',*,*,#8113,.F.);
#10835=ORIENTED_EDGE('',*,*,#8114,.F.);
#10836=ORIENTED_EDGE('',*,*,#8115,.T.);
#10837=ORIENTED_EDGE('',*,*,#8116,.F.);
#10838=ORIENTED_EDGE('',*,*,#8115,.F.);
#10839=ORIENTED_EDGE('',*,*,#8117,.F.);
#10840=ORIENTED_EDGE('',*,*,#8108,.F.);
#10841=ORIENTED_EDGE('',*,*,#8118,.F.);
#10842=ORIENTED_EDGE('',*,*,#8119,.T.);
#10843=ORIENTED_EDGE('',*,*,#8120,.F.);
#10844=ORIENTED_EDGE('',*,*,#8121,.F.);
#10845=ORIENTED_EDGE('',*,*,#8112,.F.);
#10846=ORIENTED_EDGE('',*,*,#8122,.F.);
#10847=ORIENTED_EDGE('',*,*,#8119,.F.);
#10848=ORIENTED_EDGE('',*,*,#8123,.T.);
#10849=ORIENTED_EDGE('',*,*,#8124,.T.);
#10850=ORIENTED_EDGE('',*,*,#8125,.T.);
#10851=ORIENTED_EDGE('',*,*,#8126,.T.);
#10852=ORIENTED_EDGE('',*,*,#8127,.T.);
#10853=ORIENTED_EDGE('',*,*,#8128,.T.);
#10854=ORIENTED_EDGE('',*,*,#8110,.T.);
#10855=ORIENTED_EDGE('',*,*,#8121,.T.);
#10856=ORIENTED_EDGE('',*,*,#8118,.T.);
#10857=ORIENTED_EDGE('',*,*,#8129,.T.);
#10858=ORIENTED_EDGE('',*,*,#8130,.T.);
#10859=ORIENTED_EDGE('',*,*,#8131,.T.);
#10860=ORIENTED_EDGE('',*,*,#8113,.T.);
#10861=ORIENTED_EDGE('',*,*,#8116,.T.);
#10862=ORIENTED_EDGE('',*,*,#8107,.T.);
#10863=ORIENTED_EDGE('',*,*,#8132,.T.);
#10864=ORIENTED_EDGE('',*,*,#8133,.T.);
#10865=ORIENTED_EDGE('',*,*,#8134,.T.);
#10866=ORIENTED_EDGE('',*,*,#8111,.T.);
#10867=ORIENTED_EDGE('',*,*,#8134,.F.);
#10868=ORIENTED_EDGE('',*,*,#8135,.F.);
#10869=ORIENTED_EDGE('',*,*,#8132,.F.);
#10870=ORIENTED_EDGE('',*,*,#8109,.T.);
#10871=ORIENTED_EDGE('',*,*,#8117,.T.);
#10872=ORIENTED_EDGE('',*,*,#8114,.T.);
#10873=ORIENTED_EDGE('',*,*,#8131,.F.);
#10874=ORIENTED_EDGE('',*,*,#8136,.F.);
#10875=ORIENTED_EDGE('',*,*,#8129,.F.);
#10876=ORIENTED_EDGE('',*,*,#8120,.T.);
#10877=ORIENTED_EDGE('',*,*,#8122,.T.);
#10878=ORIENTED_EDGE('',*,*,#8130,.F.);
#10879=ORIENTED_EDGE('',*,*,#8136,.T.);
#10880=ORIENTED_EDGE('',*,*,#8100,.T.);
#10881=ORIENTED_EDGE('',*,*,#8133,.F.);
#10882=ORIENTED_EDGE('',*,*,#8135,.T.);
#10883=ORIENTED_EDGE('',*,*,#8105,.T.);
#10884=ORIENTED_EDGE('',*,*,#8137,.F.);
#10885=ORIENTED_EDGE('',*,*,#8138,.T.);
#10886=ORIENTED_EDGE('',*,*,#8139,.T.);
#10887=ORIENTED_EDGE('',*,*,#8140,.F.);
#10888=ORIENTED_EDGE('',*,*,#8141,.F.);
#10889=ORIENTED_EDGE('',*,*,#8142,.T.);
#10890=ORIENTED_EDGE('',*,*,#8143,.T.);
#10891=ORIENTED_EDGE('',*,*,#8138,.F.);
#10892=ORIENTED_EDGE('',*,*,#8144,.F.);
#10893=ORIENTED_EDGE('',*,*,#8145,.T.);
#10894=ORIENTED_EDGE('',*,*,#8146,.T.);
#10895=ORIENTED_EDGE('',*,*,#8142,.F.);
#10896=ORIENTED_EDGE('',*,*,#8147,.F.);
#10897=ORIENTED_EDGE('',*,*,#8140,.T.);
#10898=ORIENTED_EDGE('',*,*,#8148,.T.);
#10899=ORIENTED_EDGE('',*,*,#8145,.F.);
#10900=ORIENTED_EDGE('',*,*,#8148,.F.);
#10901=ORIENTED_EDGE('',*,*,#8139,.F.);
#10902=ORIENTED_EDGE('',*,*,#8143,.F.);
#10903=ORIENTED_EDGE('',*,*,#8146,.F.);
#10904=ORIENTED_EDGE('',*,*,#8149,.F.);
#10905=ORIENTED_EDGE('',*,*,#8150,.T.);
#10906=ORIENTED_EDGE('',*,*,#8128,.F.);
#10907=ORIENTED_EDGE('',*,*,#8150,.F.);
#10908=ORIENTED_EDGE('',*,*,#8151,.F.);
#10909=ORIENTED_EDGE('',*,*,#8152,.T.);
#10910=ORIENTED_EDGE('',*,*,#8127,.F.);
#10911=ORIENTED_EDGE('',*,*,#8152,.F.);
#10912=ORIENTED_EDGE('',*,*,#8153,.T.);
#10913=ORIENTED_EDGE('',*,*,#8154,.T.);
#10914=ORIENTED_EDGE('',*,*,#8126,.F.);
#10915=ORIENTED_EDGE('',*,*,#8155,.F.);
#10916=ORIENTED_EDGE('',*,*,#8156,.T.);
#10917=ORIENTED_EDGE('',*,*,#8155,.T.);
#10918=ORIENTED_EDGE('',*,*,#8125,.F.);
#10919=ORIENTED_EDGE('',*,*,#8157,.F.);
#10920=ORIENTED_EDGE('',*,*,#8158,.T.);
#10921=ORIENTED_EDGE('',*,*,#8157,.T.);
#10922=ORIENTED_EDGE('',*,*,#8124,.F.);
#10923=ORIENTED_EDGE('',*,*,#8159,.F.);
#10924=ORIENTED_EDGE('',*,*,#8160,.T.);
#10925=ORIENTED_EDGE('',*,*,#8159,.T.);
#10926=ORIENTED_EDGE('',*,*,#8123,.F.);
#10927=ORIENTED_EDGE('',*,*,#8154,.F.);
#10928=ORIENTED_EDGE('',*,*,#8160,.F.);
#10929=ORIENTED_EDGE('',*,*,#8153,.F.);
#10930=ORIENTED_EDGE('',*,*,#8156,.F.);
#10931=ORIENTED_EDGE('',*,*,#8158,.F.);
#10932=ORIENTED_EDGE('',*,*,#8137,.T.);
#10933=ORIENTED_EDGE('',*,*,#8147,.T.);
#10934=ORIENTED_EDGE('',*,*,#8144,.T.);
#10935=ORIENTED_EDGE('',*,*,#8141,.T.);
#10936=ORIENTED_EDGE('',*,*,#8149,.T.);
#10937=ORIENTED_EDGE('',*,*,#8151,.T.);
#10938=ORIENTED_EDGE('',*,*,#8161,.T.);
#10939=ORIENTED_EDGE('',*,*,#8162,.T.);
#10940=ORIENTED_EDGE('',*,*,#8163,.F.);
#10941=ORIENTED_EDGE('',*,*,#8162,.F.);
#10942=ORIENTED_EDGE('',*,*,#8164,.F.);
#10943=ORIENTED_EDGE('',*,*,#8163,.T.);
#10944=ORIENTED_EDGE('',*,*,#8165,.T.);
#10945=ORIENTED_EDGE('',*,*,#8165,.F.);
#10946=ORIENTED_EDGE('',*,*,#8164,.T.);
#10947=ORIENTED_EDGE('',*,*,#8166,.F.);
#10948=ORIENTED_EDGE('',*,*,#8166,.T.);
#10949=ORIENTED_EDGE('',*,*,#8161,.F.);
#10950=ORIENTED_EDGE('',*,*,#8167,.F.);
#10951=ORIENTED_EDGE('',*,*,#8168,.F.);
#10952=ORIENTED_EDGE('',*,*,#8169,.F.);
#10953=ORIENTED_EDGE('',*,*,#8170,.T.);
#10954=ORIENTED_EDGE('',*,*,#8171,.F.);
#10955=ORIENTED_EDGE('',*,*,#8170,.F.);
#10956=ORIENTED_EDGE('',*,*,#8172,.F.);
#10957=ORIENTED_EDGE('',*,*,#8173,.T.);
#10958=ORIENTED_EDGE('',*,*,#8174,.F.);
#10959=ORIENTED_EDGE('',*,*,#8175,.F.);
#10960=ORIENTED_EDGE('',*,*,#8176,.F.);
#10961=ORIENTED_EDGE('',*,*,#8173,.F.);
#10962=ORIENTED_EDGE('',*,*,#8177,.F.);
#10963=ORIENTED_EDGE('',*,*,#8178,.T.);
#10964=ORIENTED_EDGE('',*,*,#8179,.T.);
#10965=ORIENTED_EDGE('',*,*,#8178,.F.);
#10966=ORIENTED_EDGE('',*,*,#8168,.T.);
#10967=ORIENTED_EDGE('',*,*,#8167,.T.);
#10968=ORIENTED_EDGE('',*,*,#8169,.T.);
#10969=ORIENTED_EDGE('',*,*,#8175,.T.);
#10970=ORIENTED_EDGE('',*,*,#8174,.T.);
#10971=ORIENTED_EDGE('',*,*,#8176,.T.);
#10972=ORIENTED_EDGE('',*,*,#8180,.T.);
#10973=ORIENTED_EDGE('',*,*,#8181,.T.);
#10974=ORIENTED_EDGE('',*,*,#8182,.T.);
#10975=ORIENTED_EDGE('',*,*,#8183,.T.);
#10976=ORIENTED_EDGE('',*,*,#8184,.T.);
#10977=ORIENTED_EDGE('',*,*,#8185,.T.);
#10978=ORIENTED_EDGE('',*,*,#8186,.T.);
#10979=ORIENTED_EDGE('',*,*,#8187,.T.);
#10980=ORIENTED_EDGE('',*,*,#8188,.T.);
#10981=ORIENTED_EDGE('',*,*,#8189,.T.);
#10982=ORIENTED_EDGE('',*,*,#8190,.T.);
#10983=ORIENTED_EDGE('',*,*,#8191,.T.);
#10984=ORIENTED_EDGE('',*,*,#8181,.F.);
#10985=ORIENTED_EDGE('',*,*,#8180,.F.);
#10986=ORIENTED_EDGE('',*,*,#8182,.F.);
#10987=ORIENTED_EDGE('',*,*,#8192,.T.);
#10988=ORIENTED_EDGE('',*,*,#8193,.F.);
#10989=ORIENTED_EDGE('',*,*,#8192,.F.);
#10990=ORIENTED_EDGE('',*,*,#8194,.F.);
#10991=ORIENTED_EDGE('',*,*,#8195,.T.);
#10992=ORIENTED_EDGE('',*,*,#8184,.F.);
#10993=ORIENTED_EDGE('',*,*,#8183,.F.);
#10994=ORIENTED_EDGE('',*,*,#8185,.F.);
#10995=ORIENTED_EDGE('',*,*,#8195,.F.);
#10996=ORIENTED_EDGE('',*,*,#8187,.F.);
#10997=ORIENTED_EDGE('',*,*,#8186,.F.);
#10998=ORIENTED_EDGE('',*,*,#8188,.F.);
#10999=ORIENTED_EDGE('',*,*,#8196,.T.);
#11000=ORIENTED_EDGE('',*,*,#8197,.F.);
#11001=ORIENTED_EDGE('',*,*,#8196,.F.);
#11002=ORIENTED_EDGE('',*,*,#8198,.F.);
#11003=ORIENTED_EDGE('',*,*,#8199,.T.);
#11004=ORIENTED_EDGE('',*,*,#8190,.F.);
#11005=ORIENTED_EDGE('',*,*,#8189,.F.);
#11006=ORIENTED_EDGE('',*,*,#8191,.F.);
#11007=ORIENTED_EDGE('',*,*,#8199,.F.);
#11008=ORIENTED_EDGE('',*,*,#8179,.F.);
#11009=ORIENTED_EDGE('',*,*,#8200,.T.);
#11010=ORIENTED_EDGE('',*,*,#8201,.F.);
#11011=ORIENTED_EDGE('',*,*,#8177,.T.);
#11012=ORIENTED_EDGE('',*,*,#8202,.F.);
#11013=ORIENTED_EDGE('',*,*,#8203,.T.);
#11014=ORIENTED_EDGE('',*,*,#8201,.T.);
#11015=ORIENTED_EDGE('',*,*,#8203,.F.);
#11016=ORIENTED_EDGE('',*,*,#8202,.T.);
#11017=ORIENTED_EDGE('',*,*,#8204,.F.);
#11018=ORIENTED_EDGE('',*,*,#8204,.T.);
#11019=ORIENTED_EDGE('',*,*,#8205,.T.);
#11020=ORIENTED_EDGE('',*,*,#8200,.F.);
#11021=ORIENTED_EDGE('',*,*,#8205,.F.);
#11022=ORIENTED_EDGE('',*,*,#8172,.T.);
#11023=ORIENTED_EDGE('',*,*,#8171,.T.);
#11024=ORIENTED_EDGE('',*,*,#8194,.T.);
#11025=ORIENTED_EDGE('',*,*,#8193,.T.);
#11026=ORIENTED_EDGE('',*,*,#8198,.T.);
#11027=ORIENTED_EDGE('',*,*,#8197,.T.);
#11028=ORIENTED_EDGE('',*,*,#8206,.F.);
#11029=ORIENTED_EDGE('',*,*,#8207,.T.);
#11030=ORIENTED_EDGE('',*,*,#8208,.T.);
#11031=ORIENTED_EDGE('',*,*,#8207,.F.);
#11032=ORIENTED_EDGE('',*,*,#8209,.F.);
#11033=ORIENTED_EDGE('',*,*,#8210,.T.);
#11034=ORIENTED_EDGE('',*,*,#8211,.T.);
#11035=ORIENTED_EDGE('',*,*,#8210,.F.);
#11036=ORIENTED_EDGE('',*,*,#8209,.T.);
#11037=ORIENTED_EDGE('',*,*,#8206,.T.);
#11038=ORIENTED_EDGE('',*,*,#8211,.F.);
#11039=ORIENTED_EDGE('',*,*,#8208,.F.);
#11040=ORIENTED_EDGE('',*,*,#8212,.T.);
#11041=ORIENTED_EDGE('',*,*,#8213,.T.);
#11042=ORIENTED_EDGE('',*,*,#8214,.T.);
#11043=ORIENTED_EDGE('',*,*,#8215,.F.);
#11044=ORIENTED_EDGE('',*,*,#8216,.T.);
#11045=ORIENTED_EDGE('',*,*,#8217,.T.);
#11046=ORIENTED_EDGE('',*,*,#8218,.T.);
#11047=ORIENTED_EDGE('',*,*,#8213,.F.);
#11048=ORIENTED_EDGE('',*,*,#8219,.T.);
#11049=ORIENTED_EDGE('',*,*,#8220,.T.);
#11050=ORIENTED_EDGE('',*,*,#8221,.T.);
#11051=ORIENTED_EDGE('',*,*,#8217,.F.);
#11052=ORIENTED_EDGE('',*,*,#8222,.T.);
#11053=ORIENTED_EDGE('',*,*,#8223,.T.);
#11054=ORIENTED_EDGE('',*,*,#8224,.T.);
#11055=ORIENTED_EDGE('',*,*,#8220,.F.);
#11056=ORIENTED_EDGE('',*,*,#8225,.T.);
#11057=ORIENTED_EDGE('',*,*,#8226,.T.);
#11058=ORIENTED_EDGE('',*,*,#8227,.T.);
#11059=ORIENTED_EDGE('',*,*,#8223,.F.);
#11060=ORIENTED_EDGE('',*,*,#8228,.T.);
#11061=ORIENTED_EDGE('',*,*,#8215,.T.);
#11062=ORIENTED_EDGE('',*,*,#8229,.T.);
#11063=ORIENTED_EDGE('',*,*,#8226,.F.);
#11064=ORIENTED_EDGE('',*,*,#8228,.F.);
#11065=ORIENTED_EDGE('',*,*,#8225,.F.);
#11066=ORIENTED_EDGE('',*,*,#8222,.F.);
#11067=ORIENTED_EDGE('',*,*,#8219,.F.);
#11068=ORIENTED_EDGE('',*,*,#8216,.F.);
#11069=ORIENTED_EDGE('',*,*,#8212,.F.);
#11070=ORIENTED_EDGE('',*,*,#8229,.F.);
#11071=ORIENTED_EDGE('',*,*,#8214,.F.);
#11072=ORIENTED_EDGE('',*,*,#8218,.F.);
#11073=ORIENTED_EDGE('',*,*,#8221,.F.);
#11074=ORIENTED_EDGE('',*,*,#8224,.F.);
#11075=ORIENTED_EDGE('',*,*,#8227,.F.);
#11076=ORIENTED_EDGE('',*,*,#8230,.F.);
#11077=ORIENTED_EDGE('',*,*,#8231,.F.);
#11078=ORIENTED_EDGE('',*,*,#8232,.F.);
#11079=ORIENTED_EDGE('',*,*,#8233,.T.);
#11080=ORIENTED_EDGE('',*,*,#8231,.T.);
#11081=ORIENTED_EDGE('',*,*,#8233,.F.);
#11082=ORIENTED_EDGE('',*,*,#8234,.F.);
#11083=ORIENTED_EDGE('',*,*,#8235,.T.);
#11084=ORIENTED_EDGE('',*,*,#8232,.T.);
#11085=ORIENTED_EDGE('',*,*,#8235,.F.);
#11086=ORIENTED_EDGE('',*,*,#8236,.F.);
#11087=ORIENTED_EDGE('',*,*,#8237,.T.);
#11088=ORIENTED_EDGE('',*,*,#8234,.T.);
#11089=ORIENTED_EDGE('',*,*,#8237,.F.);
#11090=ORIENTED_EDGE('',*,*,#8236,.T.);
#11091=ORIENTED_EDGE('',*,*,#8238,.F.);
#11092=ORIENTED_EDGE('',*,*,#8239,.F.);
#11093=ORIENTED_EDGE('',*,*,#8240,.T.);
#11094=ORIENTED_EDGE('',*,*,#8238,.T.);
#11095=ORIENTED_EDGE('',*,*,#8240,.F.);
#11096=ORIENTED_EDGE('',*,*,#8230,.T.);
#11097=ORIENTED_EDGE('',*,*,#8241,.T.);
#11098=ORIENTED_EDGE('',*,*,#8239,.T.);
#11099=ORIENTED_EDGE('',*,*,#8241,.F.);
#11100=ORIENTED_EDGE('',*,*,#8242,.T.);
#11101=ORIENTED_EDGE('',*,*,#8243,.T.);
#11102=ORIENTED_EDGE('',*,*,#8244,.T.);
#11103=ORIENTED_EDGE('',*,*,#8245,.F.);
#11104=ORIENTED_EDGE('',*,*,#8246,.T.);
#11105=ORIENTED_EDGE('',*,*,#8247,.T.);
#11106=ORIENTED_EDGE('',*,*,#8248,.T.);
#11107=ORIENTED_EDGE('',*,*,#8243,.F.);
#11108=ORIENTED_EDGE('',*,*,#8249,.T.);
#11109=ORIENTED_EDGE('',*,*,#8250,.T.);
#11110=ORIENTED_EDGE('',*,*,#8251,.T.);
#11111=ORIENTED_EDGE('',*,*,#8247,.F.);
#11112=ORIENTED_EDGE('',*,*,#8252,.T.);
#11113=ORIENTED_EDGE('',*,*,#8253,.T.);
#11114=ORIENTED_EDGE('',*,*,#8254,.T.);
#11115=ORIENTED_EDGE('',*,*,#8250,.F.);
#11116=ORIENTED_EDGE('',*,*,#8255,.T.);
#11117=ORIENTED_EDGE('',*,*,#8256,.T.);
#11118=ORIENTED_EDGE('',*,*,#8257,.T.);
#11119=ORIENTED_EDGE('',*,*,#8253,.F.);
#11120=ORIENTED_EDGE('',*,*,#8258,.T.);
#11121=ORIENTED_EDGE('',*,*,#8245,.T.);
#11122=ORIENTED_EDGE('',*,*,#8259,.T.);
#11123=ORIENTED_EDGE('',*,*,#8256,.F.);
#11124=ORIENTED_EDGE('',*,*,#8258,.F.);
#11125=ORIENTED_EDGE('',*,*,#8255,.F.);
#11126=ORIENTED_EDGE('',*,*,#8252,.F.);
#11127=ORIENTED_EDGE('',*,*,#8249,.F.);
#11128=ORIENTED_EDGE('',*,*,#8246,.F.);
#11129=ORIENTED_EDGE('',*,*,#8242,.F.);
#11130=ORIENTED_EDGE('',*,*,#8259,.F.);
#11131=ORIENTED_EDGE('',*,*,#8244,.F.);
#11132=ORIENTED_EDGE('',*,*,#8248,.F.);
#11133=ORIENTED_EDGE('',*,*,#8251,.F.);
#11134=ORIENTED_EDGE('',*,*,#8254,.F.);
#11135=ORIENTED_EDGE('',*,*,#8257,.F.);
#11136=ORIENTED_EDGE('',*,*,#8260,.F.);
#11137=ORIENTED_EDGE('',*,*,#8261,.F.);
#11138=ORIENTED_EDGE('',*,*,#8262,.F.);
#11139=ORIENTED_EDGE('',*,*,#8263,.T.);
#11140=ORIENTED_EDGE('',*,*,#8261,.T.);
#11141=ORIENTED_EDGE('',*,*,#8263,.F.);
#11142=ORIENTED_EDGE('',*,*,#8264,.F.);
#11143=ORIENTED_EDGE('',*,*,#8265,.T.);
#11144=ORIENTED_EDGE('',*,*,#8262,.T.);
#11145=ORIENTED_EDGE('',*,*,#8265,.F.);
#11146=ORIENTED_EDGE('',*,*,#8266,.F.);
#11147=ORIENTED_EDGE('',*,*,#8267,.T.);
#11148=ORIENTED_EDGE('',*,*,#8264,.T.);
#11149=ORIENTED_EDGE('',*,*,#8267,.F.);
#11150=ORIENTED_EDGE('',*,*,#8266,.T.);
#11151=ORIENTED_EDGE('',*,*,#8268,.F.);
#11152=ORIENTED_EDGE('',*,*,#8269,.F.);
#11153=ORIENTED_EDGE('',*,*,#8270,.T.);
#11154=ORIENTED_EDGE('',*,*,#8268,.T.);
#11155=ORIENTED_EDGE('',*,*,#8270,.F.);
#11156=ORIENTED_EDGE('',*,*,#8260,.T.);
#11157=ORIENTED_EDGE('',*,*,#8271,.T.);
#11158=ORIENTED_EDGE('',*,*,#8269,.T.);
#11159=ORIENTED_EDGE('',*,*,#8271,.F.);
#11160=ORIENTED_EDGE('',*,*,#8272,.F.);
#11161=ORIENTED_EDGE('',*,*,#8273,.T.);
#11162=ORIENTED_EDGE('',*,*,#8274,.T.);
#11163=ORIENTED_EDGE('',*,*,#8273,.F.);
#11164=ORIENTED_EDGE('',*,*,#8274,.F.);
#11165=ORIENTED_EDGE('',*,*,#8275,.T.);
#11166=ORIENTED_EDGE('',*,*,#8276,.F.);
#11167=ORIENTED_EDGE('',*,*,#8277,.F.);
#11168=ORIENTED_EDGE('',*,*,#8278,.F.);
#11169=ORIENTED_EDGE('',*,*,#8275,.F.);
#11170=ORIENTED_EDGE('',*,*,#8279,.T.);
#11171=ORIENTED_EDGE('',*,*,#8277,.T.);
#11172=ORIENTED_EDGE('',*,*,#8279,.F.);
#11173=ORIENTED_EDGE('',*,*,#8278,.T.);
#11174=ORIENTED_EDGE('',*,*,#8280,.T.);
#11175=ORIENTED_EDGE('',*,*,#8281,.T.);
#11176=ORIENTED_EDGE('',*,*,#8280,.F.);
#11177=ORIENTED_EDGE('',*,*,#8282,.F.);
#11178=ORIENTED_EDGE('',*,*,#8283,.T.);
#11179=ORIENTED_EDGE('',*,*,#8284,.T.);
#11180=ORIENTED_EDGE('',*,*,#8283,.F.);
#11181=ORIENTED_EDGE('',*,*,#8284,.F.);
#11182=ORIENTED_EDGE('',*,*,#8272,.T.);
#11183=ORIENTED_EDGE('',*,*,#8285,.F.);
#11184=ORIENTED_EDGE('',*,*,#8286,.T.);
#11185=ORIENTED_EDGE('',*,*,#8276,.T.);
#11186=ORIENTED_EDGE('',*,*,#8286,.F.);
#11187=ORIENTED_EDGE('',*,*,#8285,.T.);
#11188=ORIENTED_EDGE('',*,*,#8281,.F.);
#11189=ORIENTED_EDGE('',*,*,#8282,.T.);
#11190=ORIENTED_EDGE('',*,*,#8287,.F.);
#11191=ORIENTED_EDGE('',*,*,#8288,.T.);
#11192=ORIENTED_EDGE('',*,*,#8289,.F.);
#11193=ORIENTED_EDGE('',*,*,#8288,.F.);
#11194=ORIENTED_EDGE('',*,*,#8287,.T.);
#11195=ORIENTED_EDGE('',*,*,#8290,.F.);
#11196=ORIENTED_EDGE('',*,*,#8290,.T.);
#11197=ORIENTED_EDGE('',*,*,#8291,.T.);
#11198=ORIENTED_EDGE('',*,*,#8292,.T.);
#11199=ORIENTED_EDGE('',*,*,#8291,.F.);
#11200=ORIENTED_EDGE('',*,*,#8293,.F.);
#11201=ORIENTED_EDGE('',*,*,#8294,.T.);
#11202=ORIENTED_EDGE('',*,*,#8295,.T.);
#11203=ORIENTED_EDGE('',*,*,#8294,.F.);
#11204=ORIENTED_EDGE('',*,*,#8293,.T.);
#11205=ORIENTED_EDGE('',*,*,#8289,.T.);
#11206=ORIENTED_EDGE('',*,*,#8295,.F.);
#11207=ORIENTED_EDGE('',*,*,#8292,.F.);
#11208=ORIENTED_EDGE('',*,*,#8296,.F.);
#11209=ORIENTED_EDGE('',*,*,#8297,.T.);
#11210=ORIENTED_EDGE('',*,*,#8298,.T.);
#11211=ORIENTED_EDGE('',*,*,#8297,.F.);
#11212=ORIENTED_EDGE('',*,*,#8299,.F.);
#11213=ORIENTED_EDGE('',*,*,#8300,.T.);
#11214=ORIENTED_EDGE('',*,*,#8301,.T.);
#11215=ORIENTED_EDGE('',*,*,#8300,.F.);
#11216=ORIENTED_EDGE('',*,*,#8299,.T.);
#11217=ORIENTED_EDGE('',*,*,#8296,.T.);
#11218=ORIENTED_EDGE('',*,*,#8301,.F.);
#11219=ORIENTED_EDGE('',*,*,#8298,.F.);
#11220=ORIENTED_EDGE('',*,*,#8302,.F.);
#11221=ORIENTED_EDGE('',*,*,#8303,.T.);
#11222=ORIENTED_EDGE('',*,*,#8304,.T.);
#11223=ORIENTED_EDGE('',*,*,#8303,.F.);
#11224=ORIENTED_EDGE('',*,*,#8302,.T.);
#11225=ORIENTED_EDGE('',*,*,#8304,.F.);
#11226=ORIENTED_EDGE('',*,*,#8305,.F.);
#11227=ORIENTED_EDGE('',*,*,#8306,.T.);
#11228=ORIENTED_EDGE('',*,*,#8307,.T.);
#11229=ORIENTED_EDGE('',*,*,#8306,.F.);
#11230=ORIENTED_EDGE('',*,*,#8305,.T.);
#11231=ORIENTED_EDGE('',*,*,#8307,.F.);
#11232=ORIENTED_EDGE('',*,*,#8308,.F.);
#11233=ORIENTED_EDGE('',*,*,#8309,.T.);
#11234=ORIENTED_EDGE('',*,*,#8310,.T.);
#11235=ORIENTED_EDGE('',*,*,#8309,.F.);
#11236=ORIENTED_EDGE('',*,*,#8311,.F.);
#11237=ORIENTED_EDGE('',*,*,#8312,.T.);
#11238=ORIENTED_EDGE('',*,*,#8313,.T.);
#11239=ORIENTED_EDGE('',*,*,#8312,.F.);
#11240=ORIENTED_EDGE('',*,*,#8311,.T.);
#11241=ORIENTED_EDGE('',*,*,#8308,.T.);
#11242=ORIENTED_EDGE('',*,*,#8313,.F.);
#11243=ORIENTED_EDGE('',*,*,#8310,.F.);
#11244=ORIENTED_EDGE('',*,*,#8314,.F.);
#11245=ORIENTED_EDGE('',*,*,#8315,.T.);
#11246=ORIENTED_EDGE('',*,*,#8316,.T.);
#11247=ORIENTED_EDGE('',*,*,#8315,.F.);
#11248=ORIENTED_EDGE('',*,*,#8314,.T.);
#11249=ORIENTED_EDGE('',*,*,#8316,.F.);
#11250=ORIENTED_EDGE('',*,*,#8317,.F.);
#11251=ORIENTED_EDGE('',*,*,#8318,.T.);
#11252=ORIENTED_EDGE('',*,*,#8319,.F.);
#11253=ORIENTED_EDGE('',*,*,#8320,.F.);
#11254=ORIENTED_EDGE('',*,*,#8321,.T.);
#11255=ORIENTED_EDGE('',*,*,#8322,.F.);
#11256=ORIENTED_EDGE('',*,*,#8323,.F.);
#11257=ORIENTED_EDGE('',*,*,#8321,.F.);
#11258=ORIENTED_EDGE('',*,*,#8324,.F.);
#11259=ORIENTED_EDGE('',*,*,#8325,.F.);
#11260=ORIENTED_EDGE('',*,*,#8318,.F.);
#11261=ORIENTED_EDGE('',*,*,#8326,.F.);
#11262=ORIENTED_EDGE('',*,*,#8324,.T.);
#11263=ORIENTED_EDGE('',*,*,#8320,.T.);
#11264=ORIENTED_EDGE('',*,*,#8327,.F.);
#11265=ORIENTED_EDGE('',*,*,#8328,.T.);
#11266=ORIENTED_EDGE('',*,*,#8329,.F.);
#11267=ORIENTED_EDGE('',*,*,#8330,.F.);
#11268=ORIENTED_EDGE('',*,*,#8331,.T.);
#11269=ORIENTED_EDGE('',*,*,#8332,.F.);
#11270=ORIENTED_EDGE('',*,*,#8333,.F.);
#11271=ORIENTED_EDGE('',*,*,#8331,.F.);
#11272=ORIENTED_EDGE('',*,*,#8334,.F.);
#11273=ORIENTED_EDGE('',*,*,#8335,.F.);
#11274=ORIENTED_EDGE('',*,*,#8328,.F.);
#11275=ORIENTED_EDGE('',*,*,#8336,.F.);
#11276=ORIENTED_EDGE('',*,*,#8334,.T.);
#11277=ORIENTED_EDGE('',*,*,#8330,.T.);
#11278=ORIENTED_EDGE('',*,*,#8337,.F.);
#11279=ORIENTED_EDGE('',*,*,#8338,.T.);
#11280=ORIENTED_EDGE('',*,*,#8339,.T.);
#11281=ORIENTED_EDGE('',*,*,#8338,.F.);
#11282=ORIENTED_EDGE('',*,*,#8325,.T.);
#11283=ORIENTED_EDGE('',*,*,#8326,.T.);
#11284=ORIENTED_EDGE('',*,*,#8319,.T.);
#11285=ORIENTED_EDGE('',*,*,#8317,.T.);
#11286=ORIENTED_EDGE('',*,*,#8335,.T.);
#11287=ORIENTED_EDGE('',*,*,#8336,.T.);
#11288=ORIENTED_EDGE('',*,*,#8329,.T.);
#11289=ORIENTED_EDGE('',*,*,#8327,.T.);
#11290=ORIENTED_EDGE('',*,*,#8340,.F.);
#11291=ORIENTED_EDGE('',*,*,#8341,.T.);
#11292=ORIENTED_EDGE('',*,*,#8342,.T.);
#11293=ORIENTED_EDGE('',*,*,#8341,.F.);
#11294=ORIENTED_EDGE('',*,*,#8322,.T.);
#11295=ORIENTED_EDGE('',*,*,#8323,.T.);
#11296=ORIENTED_EDGE('',*,*,#8332,.T.);
#11297=ORIENTED_EDGE('',*,*,#8333,.T.);
#11298=ORIENTED_EDGE('',*,*,#8340,.T.);
#11299=ORIENTED_EDGE('',*,*,#8337,.T.);
#11300=ORIENTED_EDGE('',*,*,#8342,.F.);
#11301=ORIENTED_EDGE('',*,*,#8339,.F.);
#11302=ORIENTED_EDGE('',*,*,#8343,.F.);
#11303=ORIENTED_EDGE('',*,*,#8344,.F.);
#11304=ORIENTED_EDGE('',*,*,#8345,.F.);
#11305=ORIENTED_EDGE('',*,*,#8346,.T.);
#11306=ORIENTED_EDGE('',*,*,#8347,.F.);
#11307=ORIENTED_EDGE('',*,*,#8348,.F.);
#11308=ORIENTED_EDGE('',*,*,#8349,.F.);
#11309=ORIENTED_EDGE('',*,*,#8350,.F.);
#11310=ORIENTED_EDGE('',*,*,#8346,.F.);
#11311=ORIENTED_EDGE('',*,*,#8351,.F.);
#11312=ORIENTED_EDGE('',*,*,#8352,.F.);
#11313=ORIENTED_EDGE('',*,*,#8353,.T.);
#11314=ORIENTED_EDGE('',*,*,#8354,.F.);
#11315=ORIENTED_EDGE('',*,*,#8355,.F.);
#11316=ORIENTED_EDGE('',*,*,#8356,.F.);
#11317=ORIENTED_EDGE('',*,*,#8353,.F.);
#11318=ORIENTED_EDGE('',*,*,#8357,.F.);
#11319=ORIENTED_EDGE('',*,*,#8358,.T.);
#11320=ORIENTED_EDGE('',*,*,#8344,.T.);
#11321=ORIENTED_EDGE('',*,*,#8359,.T.);
#11322=ORIENTED_EDGE('',*,*,#8360,.F.);
#11323=ORIENTED_EDGE('',*,*,#8359,.F.);
#11324=ORIENTED_EDGE('',*,*,#8343,.T.);
#11325=ORIENTED_EDGE('',*,*,#8345,.T.);
#11326=ORIENTED_EDGE('',*,*,#8358,.F.);
#11327=ORIENTED_EDGE('',*,*,#8355,.T.);
#11328=ORIENTED_EDGE('',*,*,#8354,.T.);
#11329=ORIENTED_EDGE('',*,*,#8356,.T.);
#11330=ORIENTED_EDGE('',*,*,#8361,.T.);
#11331=ORIENTED_EDGE('',*,*,#8362,.T.);
#11332=ORIENTED_EDGE('',*,*,#8363,.T.);
#11333=ORIENTED_EDGE('',*,*,#8364,.T.);
#11334=ORIENTED_EDGE('',*,*,#8365,.T.);
#11335=ORIENTED_EDGE('',*,*,#8366,.T.);
#11336=ORIENTED_EDGE('',*,*,#8362,.F.);
#11337=ORIENTED_EDGE('',*,*,#8361,.F.);
#11338=ORIENTED_EDGE('',*,*,#8363,.F.);
#11339=ORIENTED_EDGE('',*,*,#8367,.T.);
#11340=ORIENTED_EDGE('',*,*,#8368,.F.);
#11341=ORIENTED_EDGE('',*,*,#8369,.F.);
#11342=ORIENTED_EDGE('',*,*,#8367,.F.);
#11343=ORIENTED_EDGE('',*,*,#8370,.F.);
#11344=ORIENTED_EDGE('',*,*,#8371,.F.);
#11345=ORIENTED_EDGE('',*,*,#8372,.T.);
#11346=ORIENTED_EDGE('',*,*,#8365,.F.);
#11347=ORIENTED_EDGE('',*,*,#8364,.F.);
#11348=ORIENTED_EDGE('',*,*,#8366,.F.);
#11349=ORIENTED_EDGE('',*,*,#8372,.F.);
#11350=ORIENTED_EDGE('',*,*,#8373,.F.);
#11351=ORIENTED_EDGE('',*,*,#8374,.T.);
#11352=ORIENTED_EDGE('',*,*,#8347,.T.);
#11353=ORIENTED_EDGE('',*,*,#8350,.T.);
#11354=ORIENTED_EDGE('',*,*,#8375,.T.);
#11355=ORIENTED_EDGE('',*,*,#8376,.F.);
#11356=ORIENTED_EDGE('',*,*,#8375,.F.);
#11357=ORIENTED_EDGE('',*,*,#8349,.T.);
#11358=ORIENTED_EDGE('',*,*,#8348,.T.);
#11359=ORIENTED_EDGE('',*,*,#8374,.F.);
#11360=ORIENTED_EDGE('',*,*,#8351,.T.);
#11361=ORIENTED_EDGE('',*,*,#8352,.T.);
#11362=ORIENTED_EDGE('',*,*,#8370,.T.);
#11363=ORIENTED_EDGE('',*,*,#8371,.T.);
#11364=ORIENTED_EDGE('',*,*,#8368,.T.);
#11365=ORIENTED_EDGE('',*,*,#8369,.T.);
#11366=ORIENTED_EDGE('',*,*,#8357,.T.);
#11367=ORIENTED_EDGE('',*,*,#8373,.T.);
#11368=ORIENTED_EDGE('',*,*,#8377,.T.);
#11369=ORIENTED_EDGE('',*,*,#8378,.T.);
#11370=ORIENTED_EDGE('',*,*,#8379,.F.);
#11371=ORIENTED_EDGE('',*,*,#8380,.T.);
#11372=ORIENTED_EDGE('',*,*,#8381,.F.);
#11373=ORIENTED_EDGE('',*,*,#8382,.T.);
#11374=ORIENTED_EDGE('',*,*,#8383,.F.);
#11375=ORIENTED_EDGE('',*,*,#8384,.T.);
#11376=ORIENTED_EDGE('',*,*,#8385,.F.);
#11377=ORIENTED_EDGE('',*,*,#8386,.T.);
#11378=ORIENTED_EDGE('',*,*,#8387,.F.);
#11379=ORIENTED_EDGE('',*,*,#8388,.T.);
#11380=ORIENTED_EDGE('',*,*,#8389,.F.);
#11381=ORIENTED_EDGE('',*,*,#8390,.T.);
#11382=ORIENTED_EDGE('',*,*,#8391,.F.);
#11383=ORIENTED_EDGE('',*,*,#8392,.T.);
#11384=ORIENTED_EDGE('',*,*,#8393,.F.);
#11385=ORIENTED_EDGE('',*,*,#8394,.T.);
#11386=ORIENTED_EDGE('',*,*,#8395,.F.);
#11387=ORIENTED_EDGE('',*,*,#8396,.T.);
#11388=ORIENTED_EDGE('',*,*,#8397,.F.);
#11389=ORIENTED_EDGE('',*,*,#8398,.T.);
#11390=ORIENTED_EDGE('',*,*,#8399,.F.);
#11391=ORIENTED_EDGE('',*,*,#8400,.T.);
#11392=ORIENTED_EDGE('',*,*,#8401,.F.);
#11393=ORIENTED_EDGE('',*,*,#8402,.T.);
#11394=ORIENTED_EDGE('',*,*,#8403,.F.);
#11395=ORIENTED_EDGE('',*,*,#8404,.T.);
#11396=ORIENTED_EDGE('',*,*,#8405,.F.);
#11397=ORIENTED_EDGE('',*,*,#8406,.T.);
#11398=ORIENTED_EDGE('',*,*,#8407,.F.);
#11399=ORIENTED_EDGE('',*,*,#8408,.T.);
#11400=ORIENTED_EDGE('',*,*,#8409,.F.);
#11401=ORIENTED_EDGE('',*,*,#8410,.T.);
#11402=ORIENTED_EDGE('',*,*,#8411,.F.);
#11403=ORIENTED_EDGE('',*,*,#8412,.T.);
#11404=ORIENTED_EDGE('',*,*,#8413,.F.);
#11405=ORIENTED_EDGE('',*,*,#8414,.T.);
#11406=ORIENTED_EDGE('',*,*,#8415,.F.);
#11407=ORIENTED_EDGE('',*,*,#8416,.T.);
#11408=ORIENTED_EDGE('',*,*,#8417,.F.);
#11409=ORIENTED_EDGE('',*,*,#8418,.F.);
#11410=ORIENTED_EDGE('',*,*,#8419,.T.);
#11411=ORIENTED_EDGE('',*,*,#8377,.F.);
#11412=ORIENTED_EDGE('',*,*,#8419,.F.);
#11413=ORIENTED_EDGE('',*,*,#8418,.T.);
#11414=ORIENTED_EDGE('',*,*,#8360,.T.);
#11415=ORIENTED_EDGE('',*,*,#8420,.F.);
#11416=ORIENTED_EDGE('',*,*,#8421,.T.);
#11417=ORIENTED_EDGE('',*,*,#8422,.T.);
#11418=ORIENTED_EDGE('',*,*,#8423,.T.);
#11419=ORIENTED_EDGE('',*,*,#8424,.T.);
#11420=ORIENTED_EDGE('',*,*,#8425,.T.);
#11421=ORIENTED_EDGE('',*,*,#8426,.T.);
#11422=ORIENTED_EDGE('',*,*,#8427,.T.);
#11423=ORIENTED_EDGE('',*,*,#8428,.T.);
#11424=ORIENTED_EDGE('',*,*,#8429,.T.);
#11425=ORIENTED_EDGE('',*,*,#8430,.T.);
#11426=ORIENTED_EDGE('',*,*,#8431,.T.);
#11427=ORIENTED_EDGE('',*,*,#8432,.T.);
#11428=ORIENTED_EDGE('',*,*,#8433,.T.);
#11429=ORIENTED_EDGE('',*,*,#8434,.T.);
#11430=ORIENTED_EDGE('',*,*,#8435,.T.);
#11431=ORIENTED_EDGE('',*,*,#8436,.T.);
#11432=ORIENTED_EDGE('',*,*,#8437,.T.);
#11433=ORIENTED_EDGE('',*,*,#8438,.T.);
#11434=ORIENTED_EDGE('',*,*,#8439,.T.);
#11435=ORIENTED_EDGE('',*,*,#8440,.T.);
#11436=ORIENTED_EDGE('',*,*,#8441,.T.);
#11437=ORIENTED_EDGE('',*,*,#8442,.T.);
#11438=ORIENTED_EDGE('',*,*,#8443,.T.);
#11439=ORIENTED_EDGE('',*,*,#8444,.T.);
#11440=ORIENTED_EDGE('',*,*,#8445,.T.);
#11441=ORIENTED_EDGE('',*,*,#8446,.T.);
#11442=ORIENTED_EDGE('',*,*,#8447,.T.);
#11443=ORIENTED_EDGE('',*,*,#8448,.T.);
#11444=ORIENTED_EDGE('',*,*,#8449,.T.);
#11445=ORIENTED_EDGE('',*,*,#8450,.T.);
#11446=ORIENTED_EDGE('',*,*,#8451,.T.);
#11447=ORIENTED_EDGE('',*,*,#8452,.T.);
#11448=ORIENTED_EDGE('',*,*,#8453,.T.);
#11449=ORIENTED_EDGE('',*,*,#8454,.T.);
#11450=ORIENTED_EDGE('',*,*,#8455,.T.);
#11451=ORIENTED_EDGE('',*,*,#8456,.T.);
#11452=ORIENTED_EDGE('',*,*,#8457,.T.);
#11453=ORIENTED_EDGE('',*,*,#8458,.T.);
#11454=ORIENTED_EDGE('',*,*,#8459,.T.);
#11455=ORIENTED_EDGE('',*,*,#8460,.T.);
#11456=ORIENTED_EDGE('',*,*,#8461,.F.);
#11457=ORIENTED_EDGE('',*,*,#8462,.T.);
#11458=ORIENTED_EDGE('',*,*,#8420,.T.);
#11459=ORIENTED_EDGE('',*,*,#8462,.F.);
#11460=ORIENTED_EDGE('',*,*,#8461,.T.);
#11461=ORIENTED_EDGE('',*,*,#8376,.T.);
#11462=ORIENTED_EDGE('',*,*,#8463,.F.);
#11463=ORIENTED_EDGE('',*,*,#8421,.F.);
#11464=ORIENTED_EDGE('',*,*,#8464,.F.);
#11465=ORIENTED_EDGE('',*,*,#8378,.F.);
#11466=ORIENTED_EDGE('',*,*,#8464,.T.);
#11467=ORIENTED_EDGE('',*,*,#8460,.F.);
#11468=ORIENTED_EDGE('',*,*,#8465,.T.);
#11469=ORIENTED_EDGE('',*,*,#8379,.T.);
#11470=ORIENTED_EDGE('',*,*,#8465,.F.);
#11471=ORIENTED_EDGE('',*,*,#8459,.F.);
#11472=ORIENTED_EDGE('',*,*,#8466,.F.);
#11473=ORIENTED_EDGE('',*,*,#8380,.F.);
#11474=ORIENTED_EDGE('',*,*,#8466,.T.);
#11475=ORIENTED_EDGE('',*,*,#8458,.F.);
#11476=ORIENTED_EDGE('',*,*,#8467,.T.);
#11477=ORIENTED_EDGE('',*,*,#8381,.T.);
#11478=ORIENTED_EDGE('',*,*,#8467,.F.);
#11479=ORIENTED_EDGE('',*,*,#8457,.F.);
#11480=ORIENTED_EDGE('',*,*,#8468,.F.);
#11481=ORIENTED_EDGE('',*,*,#8382,.F.);
#11482=ORIENTED_EDGE('',*,*,#8468,.T.);
#11483=ORIENTED_EDGE('',*,*,#8456,.F.);
#11484=ORIENTED_EDGE('',*,*,#8469,.T.);
#11485=ORIENTED_EDGE('',*,*,#8383,.T.);
#11486=ORIENTED_EDGE('',*,*,#8469,.F.);
#11487=ORIENTED_EDGE('',*,*,#8455,.F.);
#11488=ORIENTED_EDGE('',*,*,#8470,.F.);
#11489=ORIENTED_EDGE('',*,*,#8384,.F.);
#11490=ORIENTED_EDGE('',*,*,#8470,.T.);
#11491=ORIENTED_EDGE('',*,*,#8454,.F.);
#11492=ORIENTED_EDGE('',*,*,#8471,.T.);
#11493=ORIENTED_EDGE('',*,*,#8385,.T.);
#11494=ORIENTED_EDGE('',*,*,#8471,.F.);
#11495=ORIENTED_EDGE('',*,*,#8453,.F.);
#11496=ORIENTED_EDGE('',*,*,#8472,.F.);
#11497=ORIENTED_EDGE('',*,*,#8386,.F.);
#11498=ORIENTED_EDGE('',*,*,#8472,.T.);
#11499=ORIENTED_EDGE('',*,*,#8452,.F.);
#11500=ORIENTED_EDGE('',*,*,#8473,.T.);
#11501=ORIENTED_EDGE('',*,*,#8387,.T.);
#11502=ORIENTED_EDGE('',*,*,#8473,.F.);
#11503=ORIENTED_EDGE('',*,*,#8451,.F.);
#11504=ORIENTED_EDGE('',*,*,#8474,.F.);
#11505=ORIENTED_EDGE('',*,*,#8388,.F.);
#11506=ORIENTED_EDGE('',*,*,#8474,.T.);
#11507=ORIENTED_EDGE('',*,*,#8450,.F.);
#11508=ORIENTED_EDGE('',*,*,#8475,.T.);
#11509=ORIENTED_EDGE('',*,*,#8389,.T.);
#11510=ORIENTED_EDGE('',*,*,#8475,.F.);
#11511=ORIENTED_EDGE('',*,*,#8449,.F.);
#11512=ORIENTED_EDGE('',*,*,#8476,.F.);
#11513=ORIENTED_EDGE('',*,*,#8390,.F.);
#11514=ORIENTED_EDGE('',*,*,#8476,.T.);
#11515=ORIENTED_EDGE('',*,*,#8448,.F.);
#11516=ORIENTED_EDGE('',*,*,#8477,.T.);
#11517=ORIENTED_EDGE('',*,*,#8391,.T.);
#11518=ORIENTED_EDGE('',*,*,#8477,.F.);
#11519=ORIENTED_EDGE('',*,*,#8447,.F.);
#11520=ORIENTED_EDGE('',*,*,#8478,.F.);
#11521=ORIENTED_EDGE('',*,*,#8392,.F.);
#11522=ORIENTED_EDGE('',*,*,#8478,.T.);
#11523=ORIENTED_EDGE('',*,*,#8446,.F.);
#11524=ORIENTED_EDGE('',*,*,#8479,.T.);
#11525=ORIENTED_EDGE('',*,*,#8393,.T.);
#11526=ORIENTED_EDGE('',*,*,#8479,.F.);
#11527=ORIENTED_EDGE('',*,*,#8445,.F.);
#11528=ORIENTED_EDGE('',*,*,#8480,.F.);
#11529=ORIENTED_EDGE('',*,*,#8394,.F.);
#11530=ORIENTED_EDGE('',*,*,#8480,.T.);
#11531=ORIENTED_EDGE('',*,*,#8444,.F.);
#11532=ORIENTED_EDGE('',*,*,#8481,.T.);
#11533=ORIENTED_EDGE('',*,*,#8395,.T.);
#11534=ORIENTED_EDGE('',*,*,#8481,.F.);
#11535=ORIENTED_EDGE('',*,*,#8443,.F.);
#11536=ORIENTED_EDGE('',*,*,#8482,.F.);
#11537=ORIENTED_EDGE('',*,*,#8396,.F.);
#11538=ORIENTED_EDGE('',*,*,#8482,.T.);
#11539=ORIENTED_EDGE('',*,*,#8442,.F.);
#11540=ORIENTED_EDGE('',*,*,#8483,.T.);
#11541=ORIENTED_EDGE('',*,*,#8397,.T.);
#11542=ORIENTED_EDGE('',*,*,#8483,.F.);
#11543=ORIENTED_EDGE('',*,*,#8441,.F.);
#11544=ORIENTED_EDGE('',*,*,#8484,.F.);
#11545=ORIENTED_EDGE('',*,*,#8398,.F.);
#11546=ORIENTED_EDGE('',*,*,#8484,.T.);
#11547=ORIENTED_EDGE('',*,*,#8440,.F.);
#11548=ORIENTED_EDGE('',*,*,#8485,.T.);
#11549=ORIENTED_EDGE('',*,*,#8399,.T.);
#11550=ORIENTED_EDGE('',*,*,#8485,.F.);
#11551=ORIENTED_EDGE('',*,*,#8439,.F.);
#11552=ORIENTED_EDGE('',*,*,#8486,.F.);
#11553=ORIENTED_EDGE('',*,*,#8400,.F.);
#11554=ORIENTED_EDGE('',*,*,#8486,.T.);
#11555=ORIENTED_EDGE('',*,*,#8438,.F.);
#11556=ORIENTED_EDGE('',*,*,#8487,.T.);
#11557=ORIENTED_EDGE('',*,*,#8401,.T.);
#11558=ORIENTED_EDGE('',*,*,#8487,.F.);
#11559=ORIENTED_EDGE('',*,*,#8437,.F.);
#11560=ORIENTED_EDGE('',*,*,#8488,.F.);
#11561=ORIENTED_EDGE('',*,*,#8402,.F.);
#11562=ORIENTED_EDGE('',*,*,#8488,.T.);
#11563=ORIENTED_EDGE('',*,*,#8436,.F.);
#11564=ORIENTED_EDGE('',*,*,#8489,.T.);
#11565=ORIENTED_EDGE('',*,*,#8403,.T.);
#11566=ORIENTED_EDGE('',*,*,#8489,.F.);
#11567=ORIENTED_EDGE('',*,*,#8435,.F.);
#11568=ORIENTED_EDGE('',*,*,#8490,.F.);
#11569=ORIENTED_EDGE('',*,*,#8404,.F.);
#11570=ORIENTED_EDGE('',*,*,#8490,.T.);
#11571=ORIENTED_EDGE('',*,*,#8434,.F.);
#11572=ORIENTED_EDGE('',*,*,#8491,.T.);
#11573=ORIENTED_EDGE('',*,*,#8405,.T.);
#11574=ORIENTED_EDGE('',*,*,#8491,.F.);
#11575=ORIENTED_EDGE('',*,*,#8433,.F.);
#11576=ORIENTED_EDGE('',*,*,#8492,.F.);
#11577=ORIENTED_EDGE('',*,*,#8406,.F.);
#11578=ORIENTED_EDGE('',*,*,#8492,.T.);
#11579=ORIENTED_EDGE('',*,*,#8432,.F.);
#11580=ORIENTED_EDGE('',*,*,#8493,.T.);
#11581=ORIENTED_EDGE('',*,*,#8407,.T.);
#11582=ORIENTED_EDGE('',*,*,#8493,.F.);
#11583=ORIENTED_EDGE('',*,*,#8431,.F.);
#11584=ORIENTED_EDGE('',*,*,#8494,.F.);
#11585=ORIENTED_EDGE('',*,*,#8408,.F.);
#11586=ORIENTED_EDGE('',*,*,#8494,.T.);
#11587=ORIENTED_EDGE('',*,*,#8430,.F.);
#11588=ORIENTED_EDGE('',*,*,#8495,.T.);
#11589=ORIENTED_EDGE('',*,*,#8409,.T.);
#11590=ORIENTED_EDGE('',*,*,#8495,.F.);
#11591=ORIENTED_EDGE('',*,*,#8429,.F.);
#11592=ORIENTED_EDGE('',*,*,#8496,.F.);
#11593=ORIENTED_EDGE('',*,*,#8410,.F.);
#11594=ORIENTED_EDGE('',*,*,#8496,.T.);
#11595=ORIENTED_EDGE('',*,*,#8428,.F.);
#11596=ORIENTED_EDGE('',*,*,#8497,.T.);
#11597=ORIENTED_EDGE('',*,*,#8411,.T.);
#11598=ORIENTED_EDGE('',*,*,#8497,.F.);
#11599=ORIENTED_EDGE('',*,*,#8427,.F.);
#11600=ORIENTED_EDGE('',*,*,#8498,.F.);
#11601=ORIENTED_EDGE('',*,*,#8412,.F.);
#11602=ORIENTED_EDGE('',*,*,#8498,.T.);
#11603=ORIENTED_EDGE('',*,*,#8426,.F.);
#11604=ORIENTED_EDGE('',*,*,#8499,.T.);
#11605=ORIENTED_EDGE('',*,*,#8413,.T.);
#11606=ORIENTED_EDGE('',*,*,#8500,.F.);
#11607=ORIENTED_EDGE('',*,*,#8414,.F.);
#11608=ORIENTED_EDGE('',*,*,#8499,.F.);
#11609=ORIENTED_EDGE('',*,*,#8425,.F.);
#11610=ORIENTED_EDGE('',*,*,#8463,.T.);
#11611=ORIENTED_EDGE('',*,*,#8417,.T.);
#11612=ORIENTED_EDGE('',*,*,#8501,.T.);
#11613=ORIENTED_EDGE('',*,*,#8422,.F.);
#11614=ORIENTED_EDGE('',*,*,#8502,.F.);
#11615=ORIENTED_EDGE('',*,*,#8423,.F.);
#11616=ORIENTED_EDGE('',*,*,#8501,.F.);
#11617=ORIENTED_EDGE('',*,*,#8416,.F.);
#11618=ORIENTED_EDGE('',*,*,#8500,.T.);
#11619=ORIENTED_EDGE('',*,*,#8424,.F.);
#11620=ORIENTED_EDGE('',*,*,#8502,.T.);
#11621=ORIENTED_EDGE('',*,*,#8415,.T.);
#11622=ORIENTED_EDGE('',*,*,#8503,.F.);
#11623=ORIENTED_EDGE('',*,*,#8504,.T.);
#11624=ORIENTED_EDGE('',*,*,#8505,.F.);
#11625=ORIENTED_EDGE('',*,*,#8506,.T.);
#11626=ORIENTED_EDGE('',*,*,#8503,.T.);
#11627=ORIENTED_EDGE('',*,*,#8506,.F.);
#11628=ORIENTED_EDGE('',*,*,#8505,.T.);
#11629=ORIENTED_EDGE('',*,*,#8507,.F.);
#11630=ORIENTED_EDGE('',*,*,#8508,.T.);
#11631=ORIENTED_EDGE('',*,*,#8509,.T.);
#11632=ORIENTED_EDGE('',*,*,#8508,.F.);
#11633=ORIENTED_EDGE('',*,*,#8509,.F.);
#11634=ORIENTED_EDGE('',*,*,#8510,.F.);
#11635=ORIENTED_EDGE('',*,*,#8511,.F.);
#11636=ORIENTED_EDGE('',*,*,#8504,.F.);
#11637=ORIENTED_EDGE('',*,*,#8512,.T.);
#11638=ORIENTED_EDGE('',*,*,#8510,.T.);
#11639=ORIENTED_EDGE('',*,*,#8512,.F.);
#11640=ORIENTED_EDGE('',*,*,#8511,.T.);
#11641=ORIENTED_EDGE('',*,*,#8513,.T.);
#11642=ORIENTED_EDGE('',*,*,#8514,.T.);
#11643=ORIENTED_EDGE('',*,*,#8513,.F.);
#11644=ORIENTED_EDGE('',*,*,#8514,.F.);
#11645=ORIENTED_EDGE('',*,*,#8507,.T.);
#11646=ORIENTED_EDGE('',*,*,#8515,.F.);
#11647=ORIENTED_EDGE('',*,*,#8516,.T.);
#11648=ORIENTED_EDGE('',*,*,#8517,.T.);
#11649=ORIENTED_EDGE('',*,*,#8516,.F.);
#11650=ORIENTED_EDGE('',*,*,#8518,.F.);
#11651=ORIENTED_EDGE('',*,*,#8519,.T.);
#11652=ORIENTED_EDGE('',*,*,#8520,.T.);
#11653=ORIENTED_EDGE('',*,*,#8519,.F.);
#11654=ORIENTED_EDGE('',*,*,#8518,.T.);
#11655=ORIENTED_EDGE('',*,*,#8515,.T.);
#11656=ORIENTED_EDGE('',*,*,#8520,.F.);
#11657=ORIENTED_EDGE('',*,*,#8517,.F.);
#11658=ORIENTED_EDGE('',*,*,#8521,.F.);
#11659=ORIENTED_EDGE('',*,*,#8522,.T.);
#11660=ORIENTED_EDGE('',*,*,#8523,.T.);
#11661=ORIENTED_EDGE('',*,*,#8522,.F.);
#11662=ORIENTED_EDGE('',*,*,#8524,.F.);
#11663=ORIENTED_EDGE('',*,*,#8525,.T.);
#11664=ORIENTED_EDGE('',*,*,#8526,.T.);
#11665=ORIENTED_EDGE('',*,*,#8525,.F.);
#11666=ORIENTED_EDGE('',*,*,#8524,.T.);
#11667=ORIENTED_EDGE('',*,*,#8521,.T.);
#11668=ORIENTED_EDGE('',*,*,#8526,.F.);
#11669=ORIENTED_EDGE('',*,*,#8523,.F.);
#11670=ORIENTED_EDGE('',*,*,#8527,.F.);
#11671=ORIENTED_EDGE('',*,*,#8528,.T.);
#11672=ORIENTED_EDGE('',*,*,#8529,.T.);
#11673=ORIENTED_EDGE('',*,*,#8528,.F.);
#11674=ORIENTED_EDGE('',*,*,#8527,.T.);
#11675=ORIENTED_EDGE('',*,*,#8529,.F.);
#11676=ORIENTED_EDGE('',*,*,#8530,.F.);
#11677=ORIENTED_EDGE('',*,*,#8531,.T.);
#11678=ORIENTED_EDGE('',*,*,#8532,.T.);
#11679=ORIENTED_EDGE('',*,*,#8531,.F.);
#11680=ORIENTED_EDGE('',*,*,#8530,.T.);
#11681=ORIENTED_EDGE('',*,*,#8532,.F.);
#11682=ORIENTED_EDGE('',*,*,#8533,.F.);
#11683=ORIENTED_EDGE('',*,*,#8534,.T.);
#11684=ORIENTED_EDGE('',*,*,#8535,.T.);
#11685=ORIENTED_EDGE('',*,*,#8534,.F.);
#11686=ORIENTED_EDGE('',*,*,#8536,.F.);
#11687=ORIENTED_EDGE('',*,*,#8537,.T.);
#11688=ORIENTED_EDGE('',*,*,#8538,.T.);
#11689=ORIENTED_EDGE('',*,*,#8537,.F.);
#11690=ORIENTED_EDGE('',*,*,#8536,.T.);
#11691=ORIENTED_EDGE('',*,*,#8533,.T.);
#11692=ORIENTED_EDGE('',*,*,#8538,.F.);
#11693=ORIENTED_EDGE('',*,*,#8535,.F.);
#11694=ORIENTED_EDGE('',*,*,#8539,.F.);
#11695=ORIENTED_EDGE('',*,*,#8540,.T.);
#11696=ORIENTED_EDGE('',*,*,#8541,.F.);
#11697=ORIENTED_EDGE('',*,*,#8542,.F.);
#11698=ORIENTED_EDGE('',*,*,#8543,.T.);
#11699=ORIENTED_EDGE('',*,*,#8544,.F.);
#11700=ORIENTED_EDGE('',*,*,#8545,.F.);
#11701=ORIENTED_EDGE('',*,*,#8543,.F.);
#11702=ORIENTED_EDGE('',*,*,#8546,.F.);
#11703=ORIENTED_EDGE('',*,*,#8547,.F.);
#11704=ORIENTED_EDGE('',*,*,#8540,.F.);
#11705=ORIENTED_EDGE('',*,*,#8548,.F.);
#11706=ORIENTED_EDGE('',*,*,#8546,.T.);
#11707=ORIENTED_EDGE('',*,*,#8542,.T.);
#11708=ORIENTED_EDGE('',*,*,#8549,.F.);
#11709=ORIENTED_EDGE('',*,*,#8550,.T.);
#11710=ORIENTED_EDGE('',*,*,#8551,.T.);
#11711=ORIENTED_EDGE('',*,*,#8550,.F.);
#11712=ORIENTED_EDGE('',*,*,#8547,.T.);
#11713=ORIENTED_EDGE('',*,*,#8548,.T.);
#11714=ORIENTED_EDGE('',*,*,#8541,.T.);
#11715=ORIENTED_EDGE('',*,*,#8539,.T.);
#11716=ORIENTED_EDGE('',*,*,#8552,.F.);
#11717=ORIENTED_EDGE('',*,*,#8553,.T.);
#11718=ORIENTED_EDGE('',*,*,#8554,.T.);
#11719=ORIENTED_EDGE('',*,*,#8553,.F.);
#11720=ORIENTED_EDGE('',*,*,#8544,.T.);
#11721=ORIENTED_EDGE('',*,*,#8545,.T.);
#11722=ORIENTED_EDGE('',*,*,#8552,.T.);
#11723=ORIENTED_EDGE('',*,*,#8549,.T.);
#11724=ORIENTED_EDGE('',*,*,#8554,.F.);
#11725=ORIENTED_EDGE('',*,*,#8551,.F.);
#11726=ORIENTED_EDGE('',*,*,#8555,.F.);
#11727=ORIENTED_EDGE('',*,*,#8556,.T.);
#11728=ORIENTED_EDGE('',*,*,#8557,.F.);
#11729=ORIENTED_EDGE('',*,*,#8558,.F.);
#11730=ORIENTED_EDGE('',*,*,#8559,.T.);
#11731=ORIENTED_EDGE('',*,*,#8560,.F.);
#11732=ORIENTED_EDGE('',*,*,#8561,.F.);
#11733=ORIENTED_EDGE('',*,*,#8559,.F.);
#11734=ORIENTED_EDGE('',*,*,#8562,.F.);
#11735=ORIENTED_EDGE('',*,*,#8563,.F.);
#11736=ORIENTED_EDGE('',*,*,#8556,.F.);
#11737=ORIENTED_EDGE('',*,*,#8564,.F.);
#11738=ORIENTED_EDGE('',*,*,#8562,.T.);
#11739=ORIENTED_EDGE('',*,*,#8558,.T.);
#11740=ORIENTED_EDGE('',*,*,#8565,.F.);
#11741=ORIENTED_EDGE('',*,*,#8566,.T.);
#11742=ORIENTED_EDGE('',*,*,#8567,.T.);
#11743=ORIENTED_EDGE('',*,*,#8566,.F.);
#11744=ORIENTED_EDGE('',*,*,#8563,.T.);
#11745=ORIENTED_EDGE('',*,*,#8564,.T.);
#11746=ORIENTED_EDGE('',*,*,#8557,.T.);
#11747=ORIENTED_EDGE('',*,*,#8555,.T.);
#11748=ORIENTED_EDGE('',*,*,#8568,.F.);
#11749=ORIENTED_EDGE('',*,*,#8569,.T.);
#11750=ORIENTED_EDGE('',*,*,#8570,.T.);
#11751=ORIENTED_EDGE('',*,*,#8569,.F.);
#11752=ORIENTED_EDGE('',*,*,#8560,.T.);
#11753=ORIENTED_EDGE('',*,*,#8561,.T.);
#11754=ORIENTED_EDGE('',*,*,#8568,.T.);
#11755=ORIENTED_EDGE('',*,*,#8565,.T.);
#11756=ORIENTED_EDGE('',*,*,#8570,.F.);
#11757=ORIENTED_EDGE('',*,*,#8567,.F.);
#11758=ORIENTED_EDGE('',*,*,#8571,.F.);
#11759=ORIENTED_EDGE('',*,*,#8572,.T.);
#11760=ORIENTED_EDGE('',*,*,#8573,.T.);
#11761=ORIENTED_EDGE('',*,*,#8572,.F.);
#11762=ORIENTED_EDGE('',*,*,#8574,.F.);
#11763=ORIENTED_EDGE('',*,*,#8575,.T.);
#11764=ORIENTED_EDGE('',*,*,#8576,.T.);
#11765=ORIENTED_EDGE('',*,*,#8575,.F.);
#11766=ORIENTED_EDGE('',*,*,#8574,.T.);
#11767=ORIENTED_EDGE('',*,*,#8571,.T.);
#11768=ORIENTED_EDGE('',*,*,#8576,.F.);
#11769=ORIENTED_EDGE('',*,*,#8573,.F.);
#11770=ORIENTED_EDGE('',*,*,#8577,.F.);
#11771=ORIENTED_EDGE('',*,*,#8578,.T.);
#11772=ORIENTED_EDGE('',*,*,#8579,.T.);
#11773=ORIENTED_EDGE('',*,*,#8578,.F.);
#11774=ORIENTED_EDGE('',*,*,#8580,.F.);
#11775=ORIENTED_EDGE('',*,*,#8581,.T.);
#11776=ORIENTED_EDGE('',*,*,#8582,.T.);
#11777=ORIENTED_EDGE('',*,*,#8581,.F.);
#11778=ORIENTED_EDGE('',*,*,#8580,.T.);
#11779=ORIENTED_EDGE('',*,*,#8577,.T.);
#11780=ORIENTED_EDGE('',*,*,#8582,.F.);
#11781=ORIENTED_EDGE('',*,*,#8579,.F.);
#11782=ORIENTED_EDGE('',*,*,#8583,.F.);
#11783=ORIENTED_EDGE('',*,*,#8584,.T.);
#11784=ORIENTED_EDGE('',*,*,#8585,.T.);
#11785=ORIENTED_EDGE('',*,*,#8584,.F.);
#11786=ORIENTED_EDGE('',*,*,#8586,.F.);
#11787=ORIENTED_EDGE('',*,*,#8587,.T.);
#11788=ORIENTED_EDGE('',*,*,#8588,.T.);
#11789=ORIENTED_EDGE('',*,*,#8587,.F.);
#11790=ORIENTED_EDGE('',*,*,#8586,.T.);
#11791=ORIENTED_EDGE('',*,*,#8583,.T.);
#11792=ORIENTED_EDGE('',*,*,#8588,.F.);
#11793=ORIENTED_EDGE('',*,*,#8585,.F.);
#11794=ORIENTED_EDGE('',*,*,#8589,.F.);
#11795=ORIENTED_EDGE('',*,*,#8590,.T.);
#11796=ORIENTED_EDGE('',*,*,#8591,.F.);
#11797=ORIENTED_EDGE('',*,*,#8592,.F.);
#11798=ORIENTED_EDGE('',*,*,#8593,.T.);
#11799=ORIENTED_EDGE('',*,*,#8594,.F.);
#11800=ORIENTED_EDGE('',*,*,#8595,.F.);
#11801=ORIENTED_EDGE('',*,*,#8593,.F.);
#11802=ORIENTED_EDGE('',*,*,#8596,.F.);
#11803=ORIENTED_EDGE('',*,*,#8597,.F.);
#11804=ORIENTED_EDGE('',*,*,#8590,.F.);
#11805=ORIENTED_EDGE('',*,*,#8598,.F.);
#11806=ORIENTED_EDGE('',*,*,#8596,.T.);
#11807=ORIENTED_EDGE('',*,*,#8592,.T.);
#11808=ORIENTED_EDGE('',*,*,#8599,.F.);
#11809=ORIENTED_EDGE('',*,*,#8600,.T.);
#11810=ORIENTED_EDGE('',*,*,#8601,.T.);
#11811=ORIENTED_EDGE('',*,*,#8600,.F.);
#11812=ORIENTED_EDGE('',*,*,#8597,.T.);
#11813=ORIENTED_EDGE('',*,*,#8598,.T.);
#11814=ORIENTED_EDGE('',*,*,#8591,.T.);
#11815=ORIENTED_EDGE('',*,*,#8589,.T.);
#11816=ORIENTED_EDGE('',*,*,#8602,.F.);
#11817=ORIENTED_EDGE('',*,*,#8603,.T.);
#11818=ORIENTED_EDGE('',*,*,#8604,.T.);
#11819=ORIENTED_EDGE('',*,*,#8603,.F.);
#11820=ORIENTED_EDGE('',*,*,#8594,.T.);
#11821=ORIENTED_EDGE('',*,*,#8595,.T.);
#11822=ORIENTED_EDGE('',*,*,#8602,.T.);
#11823=ORIENTED_EDGE('',*,*,#8599,.T.);
#11824=ORIENTED_EDGE('',*,*,#8604,.F.);
#11825=ORIENTED_EDGE('',*,*,#8601,.F.);
#11826=ORIENTED_EDGE('',*,*,#8605,.F.);
#11827=ORIENTED_EDGE('',*,*,#8606,.T.);
#11828=ORIENTED_EDGE('',*,*,#8607,.F.);
#11829=ORIENTED_EDGE('',*,*,#8608,.F.);
#11830=ORIENTED_EDGE('',*,*,#8609,.T.);
#11831=ORIENTED_EDGE('',*,*,#8610,.F.);
#11832=ORIENTED_EDGE('',*,*,#8611,.F.);
#11833=ORIENTED_EDGE('',*,*,#8609,.F.);
#11834=ORIENTED_EDGE('',*,*,#8612,.F.);
#11835=ORIENTED_EDGE('',*,*,#8613,.F.);
#11836=ORIENTED_EDGE('',*,*,#8606,.F.);
#11837=ORIENTED_EDGE('',*,*,#8614,.F.);
#11838=ORIENTED_EDGE('',*,*,#8612,.T.);
#11839=ORIENTED_EDGE('',*,*,#8608,.T.);
#11840=ORIENTED_EDGE('',*,*,#8615,.F.);
#11841=ORIENTED_EDGE('',*,*,#8616,.T.);
#11842=ORIENTED_EDGE('',*,*,#8617,.T.);
#11843=ORIENTED_EDGE('',*,*,#8616,.F.);
#11844=ORIENTED_EDGE('',*,*,#8613,.T.);
#11845=ORIENTED_EDGE('',*,*,#8614,.T.);
#11846=ORIENTED_EDGE('',*,*,#8607,.T.);
#11847=ORIENTED_EDGE('',*,*,#8605,.T.);
#11848=ORIENTED_EDGE('',*,*,#8618,.F.);
#11849=ORIENTED_EDGE('',*,*,#8619,.T.);
#11850=ORIENTED_EDGE('',*,*,#8620,.T.);
#11851=ORIENTED_EDGE('',*,*,#8619,.F.);
#11852=ORIENTED_EDGE('',*,*,#8610,.T.);
#11853=ORIENTED_EDGE('',*,*,#8611,.T.);
#11854=ORIENTED_EDGE('',*,*,#8618,.T.);
#11855=ORIENTED_EDGE('',*,*,#8615,.T.);
#11856=ORIENTED_EDGE('',*,*,#8620,.F.);
#11857=ORIENTED_EDGE('',*,*,#8617,.F.);
#11858=ORIENTED_EDGE('',*,*,#8621,.F.);
#11859=ORIENTED_EDGE('',*,*,#8622,.F.);
#11860=ORIENTED_EDGE('',*,*,#8623,.F.);
#11861=ORIENTED_EDGE('',*,*,#8624,.T.);
#11862=ORIENTED_EDGE('',*,*,#8625,.F.);
#11863=ORIENTED_EDGE('',*,*,#8626,.F.);
#11864=ORIENTED_EDGE('',*,*,#8627,.F.);
#11865=ORIENTED_EDGE('',*,*,#8628,.F.);
#11866=ORIENTED_EDGE('',*,*,#8624,.F.);
#11867=ORIENTED_EDGE('',*,*,#8629,.F.);
#11868=ORIENTED_EDGE('',*,*,#8630,.F.);
#11869=ORIENTED_EDGE('',*,*,#8631,.T.);
#11870=ORIENTED_EDGE('',*,*,#8632,.F.);
#11871=ORIENTED_EDGE('',*,*,#8633,.F.);
#11872=ORIENTED_EDGE('',*,*,#8634,.F.);
#11873=ORIENTED_EDGE('',*,*,#8631,.F.);
#11874=ORIENTED_EDGE('',*,*,#8635,.F.);
#11875=ORIENTED_EDGE('',*,*,#8636,.T.);
#11876=ORIENTED_EDGE('',*,*,#8622,.T.);
#11877=ORIENTED_EDGE('',*,*,#8637,.T.);
#11878=ORIENTED_EDGE('',*,*,#8638,.F.);
#11879=ORIENTED_EDGE('',*,*,#8637,.F.);
#11880=ORIENTED_EDGE('',*,*,#8621,.T.);
#11881=ORIENTED_EDGE('',*,*,#8623,.T.);
#11882=ORIENTED_EDGE('',*,*,#8636,.F.);
#11883=ORIENTED_EDGE('',*,*,#8633,.T.);
#11884=ORIENTED_EDGE('',*,*,#8632,.T.);
#11885=ORIENTED_EDGE('',*,*,#8634,.T.);
#11886=ORIENTED_EDGE('',*,*,#8639,.T.);
#11887=ORIENTED_EDGE('',*,*,#8640,.T.);
#11888=ORIENTED_EDGE('',*,*,#8641,.T.);
#11889=ORIENTED_EDGE('',*,*,#8642,.T.);
#11890=ORIENTED_EDGE('',*,*,#8643,.T.);
#11891=ORIENTED_EDGE('',*,*,#8644,.T.);
#11892=ORIENTED_EDGE('',*,*,#8640,.F.);
#11893=ORIENTED_EDGE('',*,*,#8639,.F.);
#11894=ORIENTED_EDGE('',*,*,#8641,.F.);
#11895=ORIENTED_EDGE('',*,*,#8645,.T.);
#11896=ORIENTED_EDGE('',*,*,#8646,.F.);
#11897=ORIENTED_EDGE('',*,*,#8647,.F.);
#11898=ORIENTED_EDGE('',*,*,#8645,.F.);
#11899=ORIENTED_EDGE('',*,*,#8648,.F.);
#11900=ORIENTED_EDGE('',*,*,#8649,.F.);
#11901=ORIENTED_EDGE('',*,*,#8650,.T.);
#11902=ORIENTED_EDGE('',*,*,#8643,.F.);
#11903=ORIENTED_EDGE('',*,*,#8642,.F.);
#11904=ORIENTED_EDGE('',*,*,#8644,.F.);
#11905=ORIENTED_EDGE('',*,*,#8650,.F.);
#11906=ORIENTED_EDGE('',*,*,#8651,.F.);
#11907=ORIENTED_EDGE('',*,*,#8652,.T.);
#11908=ORIENTED_EDGE('',*,*,#8625,.T.);
#11909=ORIENTED_EDGE('',*,*,#8628,.T.);
#11910=ORIENTED_EDGE('',*,*,#8653,.T.);
#11911=ORIENTED_EDGE('',*,*,#8654,.F.);
#11912=ORIENTED_EDGE('',*,*,#8653,.F.);
#11913=ORIENTED_EDGE('',*,*,#8627,.T.);
#11914=ORIENTED_EDGE('',*,*,#8626,.T.);
#11915=ORIENTED_EDGE('',*,*,#8652,.F.);
#11916=ORIENTED_EDGE('',*,*,#8629,.T.);
#11917=ORIENTED_EDGE('',*,*,#8630,.T.);
#11918=ORIENTED_EDGE('',*,*,#8648,.T.);
#11919=ORIENTED_EDGE('',*,*,#8649,.T.);
#11920=ORIENTED_EDGE('',*,*,#8646,.T.);
#11921=ORIENTED_EDGE('',*,*,#8647,.T.);
#11922=ORIENTED_EDGE('',*,*,#8635,.T.);
#11923=ORIENTED_EDGE('',*,*,#8651,.T.);
#11924=ORIENTED_EDGE('',*,*,#8655,.T.);
#11925=ORIENTED_EDGE('',*,*,#8656,.T.);
#11926=ORIENTED_EDGE('',*,*,#8657,.F.);
#11927=ORIENTED_EDGE('',*,*,#8658,.T.);
#11928=ORIENTED_EDGE('',*,*,#8659,.F.);
#11929=ORIENTED_EDGE('',*,*,#8660,.T.);
#11930=ORIENTED_EDGE('',*,*,#8661,.F.);
#11931=ORIENTED_EDGE('',*,*,#8662,.T.);
#11932=ORIENTED_EDGE('',*,*,#8663,.F.);
#11933=ORIENTED_EDGE('',*,*,#8664,.T.);
#11934=ORIENTED_EDGE('',*,*,#8665,.F.);
#11935=ORIENTED_EDGE('',*,*,#8666,.T.);
#11936=ORIENTED_EDGE('',*,*,#8667,.F.);
#11937=ORIENTED_EDGE('',*,*,#8668,.T.);
#11938=ORIENTED_EDGE('',*,*,#8669,.F.);
#11939=ORIENTED_EDGE('',*,*,#8670,.T.);
#11940=ORIENTED_EDGE('',*,*,#8671,.F.);
#11941=ORIENTED_EDGE('',*,*,#8672,.T.);
#11942=ORIENTED_EDGE('',*,*,#8673,.F.);
#11943=ORIENTED_EDGE('',*,*,#8674,.T.);
#11944=ORIENTED_EDGE('',*,*,#8675,.F.);
#11945=ORIENTED_EDGE('',*,*,#8676,.T.);
#11946=ORIENTED_EDGE('',*,*,#8677,.F.);
#11947=ORIENTED_EDGE('',*,*,#8678,.T.);
#11948=ORIENTED_EDGE('',*,*,#8679,.F.);
#11949=ORIENTED_EDGE('',*,*,#8680,.T.);
#11950=ORIENTED_EDGE('',*,*,#8681,.F.);
#11951=ORIENTED_EDGE('',*,*,#8682,.T.);
#11952=ORIENTED_EDGE('',*,*,#8683,.F.);
#11953=ORIENTED_EDGE('',*,*,#8684,.T.);
#11954=ORIENTED_EDGE('',*,*,#8685,.F.);
#11955=ORIENTED_EDGE('',*,*,#8686,.T.);
#11956=ORIENTED_EDGE('',*,*,#8687,.F.);
#11957=ORIENTED_EDGE('',*,*,#8688,.T.);
#11958=ORIENTED_EDGE('',*,*,#8689,.F.);
#11959=ORIENTED_EDGE('',*,*,#8690,.T.);
#11960=ORIENTED_EDGE('',*,*,#8691,.F.);
#11961=ORIENTED_EDGE('',*,*,#8692,.T.);
#11962=ORIENTED_EDGE('',*,*,#8693,.F.);
#11963=ORIENTED_EDGE('',*,*,#8694,.T.);
#11964=ORIENTED_EDGE('',*,*,#8695,.F.);
#11965=ORIENTED_EDGE('',*,*,#8696,.T.);
#11966=ORIENTED_EDGE('',*,*,#8697,.F.);
#11967=ORIENTED_EDGE('',*,*,#8698,.T.);
#11968=ORIENTED_EDGE('',*,*,#8699,.F.);
#11969=ORIENTED_EDGE('',*,*,#8700,.T.);
#11970=ORIENTED_EDGE('',*,*,#8701,.F.);
#11971=ORIENTED_EDGE('',*,*,#8702,.T.);
#11972=ORIENTED_EDGE('',*,*,#8703,.F.);
#11973=ORIENTED_EDGE('',*,*,#8704,.T.);
#11974=ORIENTED_EDGE('',*,*,#8705,.F.);
#11975=ORIENTED_EDGE('',*,*,#8706,.T.);
#11976=ORIENTED_EDGE('',*,*,#8707,.F.);
#11977=ORIENTED_EDGE('',*,*,#8708,.T.);
#11978=ORIENTED_EDGE('',*,*,#8709,.F.);
#11979=ORIENTED_EDGE('',*,*,#8710,.T.);
#11980=ORIENTED_EDGE('',*,*,#8711,.F.);
#11981=ORIENTED_EDGE('',*,*,#8712,.T.);
#11982=ORIENTED_EDGE('',*,*,#8713,.F.);
#11983=ORIENTED_EDGE('',*,*,#8714,.T.);
#11984=ORIENTED_EDGE('',*,*,#8715,.F.);
#11985=ORIENTED_EDGE('',*,*,#8716,.T.);
#11986=ORIENTED_EDGE('',*,*,#8717,.F.);
#11987=ORIENTED_EDGE('',*,*,#8718,.T.);
#11988=ORIENTED_EDGE('',*,*,#8719,.F.);
#11989=ORIENTED_EDGE('',*,*,#8720,.T.);
#11990=ORIENTED_EDGE('',*,*,#8721,.F.);
#11991=ORIENTED_EDGE('',*,*,#8722,.T.);
#11992=ORIENTED_EDGE('',*,*,#8723,.F.);
#11993=ORIENTED_EDGE('',*,*,#8724,.T.);
#11994=ORIENTED_EDGE('',*,*,#8725,.F.);
#11995=ORIENTED_EDGE('',*,*,#8726,.T.);
#11996=ORIENTED_EDGE('',*,*,#8727,.F.);
#11997=ORIENTED_EDGE('',*,*,#8728,.T.);
#11998=ORIENTED_EDGE('',*,*,#8729,.F.);
#11999=ORIENTED_EDGE('',*,*,#8730,.T.);
#12000=ORIENTED_EDGE('',*,*,#8731,.F.);
#12001=ORIENTED_EDGE('',*,*,#8732,.T.);
#12002=ORIENTED_EDGE('',*,*,#8733,.F.);
#12003=ORIENTED_EDGE('',*,*,#8734,.T.);
#12004=ORIENTED_EDGE('',*,*,#8735,.F.);
#12005=ORIENTED_EDGE('',*,*,#8736,.F.);
#12006=ORIENTED_EDGE('',*,*,#8737,.T.);
#12007=ORIENTED_EDGE('',*,*,#8655,.F.);
#12008=ORIENTED_EDGE('',*,*,#8737,.F.);
#12009=ORIENTED_EDGE('',*,*,#8736,.T.);
#12010=ORIENTED_EDGE('',*,*,#8638,.T.);
#12011=ORIENTED_EDGE('',*,*,#8738,.F.);
#12012=ORIENTED_EDGE('',*,*,#8739,.T.);
#12013=ORIENTED_EDGE('',*,*,#8740,.T.);
#12014=ORIENTED_EDGE('',*,*,#8741,.T.);
#12015=ORIENTED_EDGE('',*,*,#8742,.T.);
#12016=ORIENTED_EDGE('',*,*,#8743,.T.);
#12017=ORIENTED_EDGE('',*,*,#8744,.T.);
#12018=ORIENTED_EDGE('',*,*,#8745,.T.);
#12019=ORIENTED_EDGE('',*,*,#8746,.T.);
#12020=ORIENTED_EDGE('',*,*,#8747,.T.);
#12021=ORIENTED_EDGE('',*,*,#8748,.T.);
#12022=ORIENTED_EDGE('',*,*,#8749,.T.);
#12023=ORIENTED_EDGE('',*,*,#8750,.T.);
#12024=ORIENTED_EDGE('',*,*,#8751,.T.);
#12025=ORIENTED_EDGE('',*,*,#8752,.T.);
#12026=ORIENTED_EDGE('',*,*,#8753,.T.);
#12027=ORIENTED_EDGE('',*,*,#8754,.T.);
#12028=ORIENTED_EDGE('',*,*,#8755,.T.);
#12029=ORIENTED_EDGE('',*,*,#8756,.T.);
#12030=ORIENTED_EDGE('',*,*,#8757,.T.);
#12031=ORIENTED_EDGE('',*,*,#8758,.T.);
#12032=ORIENTED_EDGE('',*,*,#8759,.T.);
#12033=ORIENTED_EDGE('',*,*,#8760,.T.);
#12034=ORIENTED_EDGE('',*,*,#8761,.T.);
#12035=ORIENTED_EDGE('',*,*,#8762,.T.);
#12036=ORIENTED_EDGE('',*,*,#8763,.T.);
#12037=ORIENTED_EDGE('',*,*,#8764,.T.);
#12038=ORIENTED_EDGE('',*,*,#8765,.T.);
#12039=ORIENTED_EDGE('',*,*,#8766,.T.);
#12040=ORIENTED_EDGE('',*,*,#8767,.T.);
#12041=ORIENTED_EDGE('',*,*,#8768,.T.);
#12042=ORIENTED_EDGE('',*,*,#8769,.T.);
#12043=ORIENTED_EDGE('',*,*,#8770,.T.);
#12044=ORIENTED_EDGE('',*,*,#8771,.T.);
#12045=ORIENTED_EDGE('',*,*,#8772,.T.);
#12046=ORIENTED_EDGE('',*,*,#8773,.T.);
#12047=ORIENTED_EDGE('',*,*,#8774,.T.);
#12048=ORIENTED_EDGE('',*,*,#8775,.T.);
#12049=ORIENTED_EDGE('',*,*,#8776,.T.);
#12050=ORIENTED_EDGE('',*,*,#8777,.T.);
#12051=ORIENTED_EDGE('',*,*,#8778,.T.);
#12052=ORIENTED_EDGE('',*,*,#8779,.T.);
#12053=ORIENTED_EDGE('',*,*,#8780,.T.);
#12054=ORIENTED_EDGE('',*,*,#8781,.T.);
#12055=ORIENTED_EDGE('',*,*,#8782,.T.);
#12056=ORIENTED_EDGE('',*,*,#8783,.T.);
#12057=ORIENTED_EDGE('',*,*,#8784,.T.);
#12058=ORIENTED_EDGE('',*,*,#8785,.T.);
#12059=ORIENTED_EDGE('',*,*,#8786,.T.);
#12060=ORIENTED_EDGE('',*,*,#8787,.T.);
#12061=ORIENTED_EDGE('',*,*,#8788,.T.);
#12062=ORIENTED_EDGE('',*,*,#8789,.T.);
#12063=ORIENTED_EDGE('',*,*,#8790,.T.);
#12064=ORIENTED_EDGE('',*,*,#8791,.T.);
#12065=ORIENTED_EDGE('',*,*,#8792,.T.);
#12066=ORIENTED_EDGE('',*,*,#8793,.T.);
#12067=ORIENTED_EDGE('',*,*,#8794,.T.);
#12068=ORIENTED_EDGE('',*,*,#8795,.T.);
#12069=ORIENTED_EDGE('',*,*,#8796,.T.);
#12070=ORIENTED_EDGE('',*,*,#8797,.T.);
#12071=ORIENTED_EDGE('',*,*,#8798,.T.);
#12072=ORIENTED_EDGE('',*,*,#8799,.T.);
#12073=ORIENTED_EDGE('',*,*,#8800,.T.);
#12074=ORIENTED_EDGE('',*,*,#8801,.T.);
#12075=ORIENTED_EDGE('',*,*,#8802,.T.);
#12076=ORIENTED_EDGE('',*,*,#8803,.T.);
#12077=ORIENTED_EDGE('',*,*,#8804,.T.);
#12078=ORIENTED_EDGE('',*,*,#8805,.T.);
#12079=ORIENTED_EDGE('',*,*,#8806,.T.);
#12080=ORIENTED_EDGE('',*,*,#8807,.T.);
#12081=ORIENTED_EDGE('',*,*,#8808,.T.);
#12082=ORIENTED_EDGE('',*,*,#8809,.T.);
#12083=ORIENTED_EDGE('',*,*,#8810,.T.);
#12084=ORIENTED_EDGE('',*,*,#8811,.T.);
#12085=ORIENTED_EDGE('',*,*,#8812,.T.);
#12086=ORIENTED_EDGE('',*,*,#8813,.T.);
#12087=ORIENTED_EDGE('',*,*,#8814,.T.);
#12088=ORIENTED_EDGE('',*,*,#8815,.T.);
#12089=ORIENTED_EDGE('',*,*,#8816,.T.);
#12090=ORIENTED_EDGE('',*,*,#8817,.T.);
#12091=ORIENTED_EDGE('',*,*,#8818,.T.);
#12092=ORIENTED_EDGE('',*,*,#8819,.F.);
#12093=ORIENTED_EDGE('',*,*,#8820,.T.);
#12094=ORIENTED_EDGE('',*,*,#8738,.T.);
#12095=ORIENTED_EDGE('',*,*,#8820,.F.);
#12096=ORIENTED_EDGE('',*,*,#8819,.T.);
#12097=ORIENTED_EDGE('',*,*,#8654,.T.);
#12098=ORIENTED_EDGE('',*,*,#8821,.F.);
#12099=ORIENTED_EDGE('',*,*,#8739,.F.);
#12100=ORIENTED_EDGE('',*,*,#8822,.F.);
#12101=ORIENTED_EDGE('',*,*,#8656,.F.);
#12102=ORIENTED_EDGE('',*,*,#8822,.T.);
#12103=ORIENTED_EDGE('',*,*,#8818,.F.);
#12104=ORIENTED_EDGE('',*,*,#8823,.T.);
#12105=ORIENTED_EDGE('',*,*,#8657,.T.);
#12106=ORIENTED_EDGE('',*,*,#8823,.F.);
#12107=ORIENTED_EDGE('',*,*,#8817,.F.);
#12108=ORIENTED_EDGE('',*,*,#8824,.F.);
#12109=ORIENTED_EDGE('',*,*,#8658,.F.);
#12110=ORIENTED_EDGE('',*,*,#8824,.T.);
#12111=ORIENTED_EDGE('',*,*,#8816,.F.);
#12112=ORIENTED_EDGE('',*,*,#8825,.T.);
#12113=ORIENTED_EDGE('',*,*,#8659,.T.);
#12114=ORIENTED_EDGE('',*,*,#8825,.F.);
#12115=ORIENTED_EDGE('',*,*,#8815,.F.);
#12116=ORIENTED_EDGE('',*,*,#8826,.F.);
#12117=ORIENTED_EDGE('',*,*,#8660,.F.);
#12118=ORIENTED_EDGE('',*,*,#8826,.T.);
#12119=ORIENTED_EDGE('',*,*,#8814,.F.);
#12120=ORIENTED_EDGE('',*,*,#8827,.T.);
#12121=ORIENTED_EDGE('',*,*,#8661,.T.);
#12122=ORIENTED_EDGE('',*,*,#8827,.F.);
#12123=ORIENTED_EDGE('',*,*,#8813,.F.);
#12124=ORIENTED_EDGE('',*,*,#8828,.F.);
#12125=ORIENTED_EDGE('',*,*,#8662,.F.);
#12126=ORIENTED_EDGE('',*,*,#8828,.T.);
#12127=ORIENTED_EDGE('',*,*,#8812,.F.);
#12128=ORIENTED_EDGE('',*,*,#8829,.T.);
#12129=ORIENTED_EDGE('',*,*,#8663,.T.);
#12130=ORIENTED_EDGE('',*,*,#8829,.F.);
#12131=ORIENTED_EDGE('',*,*,#8811,.F.);
#12132=ORIENTED_EDGE('',*,*,#8830,.F.);
#12133=ORIENTED_EDGE('',*,*,#8664,.F.);
#12134=ORIENTED_EDGE('',*,*,#8830,.T.);
#12135=ORIENTED_EDGE('',*,*,#8810,.F.);
#12136=ORIENTED_EDGE('',*,*,#8831,.T.);
#12137=ORIENTED_EDGE('',*,*,#8665,.T.);
#12138=ORIENTED_EDGE('',*,*,#8831,.F.);
#12139=ORIENTED_EDGE('',*,*,#8809,.F.);
#12140=ORIENTED_EDGE('',*,*,#8832,.F.);
#12141=ORIENTED_EDGE('',*,*,#8666,.F.);
#12142=ORIENTED_EDGE('',*,*,#8832,.T.);
#12143=ORIENTED_EDGE('',*,*,#8808,.F.);
#12144=ORIENTED_EDGE('',*,*,#8833,.T.);
#12145=ORIENTED_EDGE('',*,*,#8667,.T.);
#12146=ORIENTED_EDGE('',*,*,#8833,.F.);
#12147=ORIENTED_EDGE('',*,*,#8807,.F.);
#12148=ORIENTED_EDGE('',*,*,#8834,.F.);
#12149=ORIENTED_EDGE('',*,*,#8668,.F.);
#12150=ORIENTED_EDGE('',*,*,#8834,.T.);
#12151=ORIENTED_EDGE('',*,*,#8806,.F.);
#12152=ORIENTED_EDGE('',*,*,#8835,.T.);
#12153=ORIENTED_EDGE('',*,*,#8669,.T.);
#12154=ORIENTED_EDGE('',*,*,#8835,.F.);
#12155=ORIENTED_EDGE('',*,*,#8805,.F.);
#12156=ORIENTED_EDGE('',*,*,#8836,.F.);
#12157=ORIENTED_EDGE('',*,*,#8670,.F.);
#12158=ORIENTED_EDGE('',*,*,#8836,.T.);
#12159=ORIENTED_EDGE('',*,*,#8804,.F.);
#12160=ORIENTED_EDGE('',*,*,#8837,.T.);
#12161=ORIENTED_EDGE('',*,*,#8671,.T.);
#12162=ORIENTED_EDGE('',*,*,#8837,.F.);
#12163=ORIENTED_EDGE('',*,*,#8803,.F.);
#12164=ORIENTED_EDGE('',*,*,#8838,.F.);
#12165=ORIENTED_EDGE('',*,*,#8672,.F.);
#12166=ORIENTED_EDGE('',*,*,#8838,.T.);
#12167=ORIENTED_EDGE('',*,*,#8802,.F.);
#12168=ORIENTED_EDGE('',*,*,#8839,.T.);
#12169=ORIENTED_EDGE('',*,*,#8673,.T.);
#12170=ORIENTED_EDGE('',*,*,#8839,.F.);
#12171=ORIENTED_EDGE('',*,*,#8801,.F.);
#12172=ORIENTED_EDGE('',*,*,#8840,.F.);
#12173=ORIENTED_EDGE('',*,*,#8674,.F.);
#12174=ORIENTED_EDGE('',*,*,#8840,.T.);
#12175=ORIENTED_EDGE('',*,*,#8800,.F.);
#12176=ORIENTED_EDGE('',*,*,#8841,.T.);
#12177=ORIENTED_EDGE('',*,*,#8675,.T.);
#12178=ORIENTED_EDGE('',*,*,#8841,.F.);
#12179=ORIENTED_EDGE('',*,*,#8799,.F.);
#12180=ORIENTED_EDGE('',*,*,#8842,.F.);
#12181=ORIENTED_EDGE('',*,*,#8676,.F.);
#12182=ORIENTED_EDGE('',*,*,#8842,.T.);
#12183=ORIENTED_EDGE('',*,*,#8798,.F.);
#12184=ORIENTED_EDGE('',*,*,#8843,.T.);
#12185=ORIENTED_EDGE('',*,*,#8677,.T.);
#12186=ORIENTED_EDGE('',*,*,#8843,.F.);
#12187=ORIENTED_EDGE('',*,*,#8797,.F.);
#12188=ORIENTED_EDGE('',*,*,#8844,.F.);
#12189=ORIENTED_EDGE('',*,*,#8678,.F.);
#12190=ORIENTED_EDGE('',*,*,#8844,.T.);
#12191=ORIENTED_EDGE('',*,*,#8796,.F.);
#12192=ORIENTED_EDGE('',*,*,#8845,.T.);
#12193=ORIENTED_EDGE('',*,*,#8679,.T.);
#12194=ORIENTED_EDGE('',*,*,#8845,.F.);
#12195=ORIENTED_EDGE('',*,*,#8795,.F.);
#12196=ORIENTED_EDGE('',*,*,#8846,.F.);
#12197=ORIENTED_EDGE('',*,*,#8680,.F.);
#12198=ORIENTED_EDGE('',*,*,#8846,.T.);
#12199=ORIENTED_EDGE('',*,*,#8794,.F.);
#12200=ORIENTED_EDGE('',*,*,#8847,.T.);
#12201=ORIENTED_EDGE('',*,*,#8681,.T.);
#12202=ORIENTED_EDGE('',*,*,#8847,.F.);
#12203=ORIENTED_EDGE('',*,*,#8793,.F.);
#12204=ORIENTED_EDGE('',*,*,#8848,.F.);
#12205=ORIENTED_EDGE('',*,*,#8682,.F.);
#12206=ORIENTED_EDGE('',*,*,#8848,.T.);
#12207=ORIENTED_EDGE('',*,*,#8792,.F.);
#12208=ORIENTED_EDGE('',*,*,#8849,.T.);
#12209=ORIENTED_EDGE('',*,*,#8683,.T.);
#12210=ORIENTED_EDGE('',*,*,#8849,.F.);
#12211=ORIENTED_EDGE('',*,*,#8791,.F.);
#12212=ORIENTED_EDGE('',*,*,#8850,.F.);
#12213=ORIENTED_EDGE('',*,*,#8684,.F.);
#12214=ORIENTED_EDGE('',*,*,#8850,.T.);
#12215=ORIENTED_EDGE('',*,*,#8790,.F.);
#12216=ORIENTED_EDGE('',*,*,#8851,.T.);
#12217=ORIENTED_EDGE('',*,*,#8685,.T.);
#12218=ORIENTED_EDGE('',*,*,#8851,.F.);
#12219=ORIENTED_EDGE('',*,*,#8789,.F.);
#12220=ORIENTED_EDGE('',*,*,#8852,.F.);
#12221=ORIENTED_EDGE('',*,*,#8686,.F.);
#12222=ORIENTED_EDGE('',*,*,#8852,.T.);
#12223=ORIENTED_EDGE('',*,*,#8788,.F.);
#12224=ORIENTED_EDGE('',*,*,#8853,.T.);
#12225=ORIENTED_EDGE('',*,*,#8687,.T.);
#12226=ORIENTED_EDGE('',*,*,#8853,.F.);
#12227=ORIENTED_EDGE('',*,*,#8787,.F.);
#12228=ORIENTED_EDGE('',*,*,#8854,.F.);
#12229=ORIENTED_EDGE('',*,*,#8688,.F.);
#12230=ORIENTED_EDGE('',*,*,#8854,.T.);
#12231=ORIENTED_EDGE('',*,*,#8786,.F.);
#12232=ORIENTED_EDGE('',*,*,#8855,.T.);
#12233=ORIENTED_EDGE('',*,*,#8689,.T.);
#12234=ORIENTED_EDGE('',*,*,#8855,.F.);
#12235=ORIENTED_EDGE('',*,*,#8785,.F.);
#12236=ORIENTED_EDGE('',*,*,#8856,.F.);
#12237=ORIENTED_EDGE('',*,*,#8690,.F.);
#12238=ORIENTED_EDGE('',*,*,#8856,.T.);
#12239=ORIENTED_EDGE('',*,*,#8784,.F.);
#12240=ORIENTED_EDGE('',*,*,#8857,.T.);
#12241=ORIENTED_EDGE('',*,*,#8691,.T.);
#12242=ORIENTED_EDGE('',*,*,#8857,.F.);
#12243=ORIENTED_EDGE('',*,*,#8783,.F.);
#12244=ORIENTED_EDGE('',*,*,#8858,.F.);
#12245=ORIENTED_EDGE('',*,*,#8692,.F.);
#12246=ORIENTED_EDGE('',*,*,#8858,.T.);
#12247=ORIENTED_EDGE('',*,*,#8782,.F.);
#12248=ORIENTED_EDGE('',*,*,#8859,.T.);
#12249=ORIENTED_EDGE('',*,*,#8693,.T.);
#12250=ORIENTED_EDGE('',*,*,#8859,.F.);
#12251=ORIENTED_EDGE('',*,*,#8781,.F.);
#12252=ORIENTED_EDGE('',*,*,#8860,.F.);
#12253=ORIENTED_EDGE('',*,*,#8694,.F.);
#12254=ORIENTED_EDGE('',*,*,#8860,.T.);
#12255=ORIENTED_EDGE('',*,*,#8780,.F.);
#12256=ORIENTED_EDGE('',*,*,#8861,.T.);
#12257=ORIENTED_EDGE('',*,*,#8695,.T.);
#12258=ORIENTED_EDGE('',*,*,#8861,.F.);
#12259=ORIENTED_EDGE('',*,*,#8779,.F.);
#12260=ORIENTED_EDGE('',*,*,#8862,.F.);
#12261=ORIENTED_EDGE('',*,*,#8696,.F.);
#12262=ORIENTED_EDGE('',*,*,#8862,.T.);
#12263=ORIENTED_EDGE('',*,*,#8778,.F.);
#12264=ORIENTED_EDGE('',*,*,#8863,.T.);
#12265=ORIENTED_EDGE('',*,*,#8697,.T.);
#12266=ORIENTED_EDGE('',*,*,#8863,.F.);
#12267=ORIENTED_EDGE('',*,*,#8777,.F.);
#12268=ORIENTED_EDGE('',*,*,#8864,.F.);
#12269=ORIENTED_EDGE('',*,*,#8698,.F.);
#12270=ORIENTED_EDGE('',*,*,#8864,.T.);
#12271=ORIENTED_EDGE('',*,*,#8776,.F.);
#12272=ORIENTED_EDGE('',*,*,#8865,.T.);
#12273=ORIENTED_EDGE('',*,*,#8699,.T.);
#12274=ORIENTED_EDGE('',*,*,#8865,.F.);
#12275=ORIENTED_EDGE('',*,*,#8775,.F.);
#12276=ORIENTED_EDGE('',*,*,#8866,.F.);
#12277=ORIENTED_EDGE('',*,*,#8700,.F.);
#12278=ORIENTED_EDGE('',*,*,#8866,.T.);
#12279=ORIENTED_EDGE('',*,*,#8774,.F.);
#12280=ORIENTED_EDGE('',*,*,#8867,.T.);
#12281=ORIENTED_EDGE('',*,*,#8701,.T.);
#12282=ORIENTED_EDGE('',*,*,#8867,.F.);
#12283=ORIENTED_EDGE('',*,*,#8773,.F.);
#12284=ORIENTED_EDGE('',*,*,#8868,.F.);
#12285=ORIENTED_EDGE('',*,*,#8702,.F.);
#12286=ORIENTED_EDGE('',*,*,#8868,.T.);
#12287=ORIENTED_EDGE('',*,*,#8772,.F.);
#12288=ORIENTED_EDGE('',*,*,#8869,.T.);
#12289=ORIENTED_EDGE('',*,*,#8703,.T.);
#12290=ORIENTED_EDGE('',*,*,#8869,.F.);
#12291=ORIENTED_EDGE('',*,*,#8771,.F.);
#12292=ORIENTED_EDGE('',*,*,#8870,.F.);
#12293=ORIENTED_EDGE('',*,*,#8704,.F.);
#12294=ORIENTED_EDGE('',*,*,#8870,.T.);
#12295=ORIENTED_EDGE('',*,*,#8770,.F.);
#12296=ORIENTED_EDGE('',*,*,#8871,.T.);
#12297=ORIENTED_EDGE('',*,*,#8705,.T.);
#12298=ORIENTED_EDGE('',*,*,#8871,.F.);
#12299=ORIENTED_EDGE('',*,*,#8769,.F.);
#12300=ORIENTED_EDGE('',*,*,#8872,.F.);
#12301=ORIENTED_EDGE('',*,*,#8706,.F.);
#12302=ORIENTED_EDGE('',*,*,#8872,.T.);
#12303=ORIENTED_EDGE('',*,*,#8768,.F.);
#12304=ORIENTED_EDGE('',*,*,#8873,.T.);
#12305=ORIENTED_EDGE('',*,*,#8707,.T.);
#12306=ORIENTED_EDGE('',*,*,#8873,.F.);
#12307=ORIENTED_EDGE('',*,*,#8767,.F.);
#12308=ORIENTED_EDGE('',*,*,#8874,.F.);
#12309=ORIENTED_EDGE('',*,*,#8708,.F.);
#12310=ORIENTED_EDGE('',*,*,#8874,.T.);
#12311=ORIENTED_EDGE('',*,*,#8766,.F.);
#12312=ORIENTED_EDGE('',*,*,#8875,.T.);
#12313=ORIENTED_EDGE('',*,*,#8709,.T.);
#12314=ORIENTED_EDGE('',*,*,#8875,.F.);
#12315=ORIENTED_EDGE('',*,*,#8765,.F.);
#12316=ORIENTED_EDGE('',*,*,#8876,.F.);
#12317=ORIENTED_EDGE('',*,*,#8710,.F.);
#12318=ORIENTED_EDGE('',*,*,#8876,.T.);
#12319=ORIENTED_EDGE('',*,*,#8764,.F.);
#12320=ORIENTED_EDGE('',*,*,#8877,.T.);
#12321=ORIENTED_EDGE('',*,*,#8711,.T.);
#12322=ORIENTED_EDGE('',*,*,#8877,.F.);
#12323=ORIENTED_EDGE('',*,*,#8763,.F.);
#12324=ORIENTED_EDGE('',*,*,#8878,.F.);
#12325=ORIENTED_EDGE('',*,*,#8712,.F.);
#12326=ORIENTED_EDGE('',*,*,#8878,.T.);
#12327=ORIENTED_EDGE('',*,*,#8762,.F.);
#12328=ORIENTED_EDGE('',*,*,#8879,.T.);
#12329=ORIENTED_EDGE('',*,*,#8713,.T.);
#12330=ORIENTED_EDGE('',*,*,#8879,.F.);
#12331=ORIENTED_EDGE('',*,*,#8761,.F.);
#12332=ORIENTED_EDGE('',*,*,#8880,.F.);
#12333=ORIENTED_EDGE('',*,*,#8714,.F.);
#12334=ORIENTED_EDGE('',*,*,#8880,.T.);
#12335=ORIENTED_EDGE('',*,*,#8760,.F.);
#12336=ORIENTED_EDGE('',*,*,#8881,.T.);
#12337=ORIENTED_EDGE('',*,*,#8715,.T.);
#12338=ORIENTED_EDGE('',*,*,#8881,.F.);
#12339=ORIENTED_EDGE('',*,*,#8759,.F.);
#12340=ORIENTED_EDGE('',*,*,#8882,.F.);
#12341=ORIENTED_EDGE('',*,*,#8716,.F.);
#12342=ORIENTED_EDGE('',*,*,#8882,.T.);
#12343=ORIENTED_EDGE('',*,*,#8758,.F.);
#12344=ORIENTED_EDGE('',*,*,#8883,.T.);
#12345=ORIENTED_EDGE('',*,*,#8717,.T.);
#12346=ORIENTED_EDGE('',*,*,#8883,.F.);
#12347=ORIENTED_EDGE('',*,*,#8757,.F.);
#12348=ORIENTED_EDGE('',*,*,#8884,.F.);
#12349=ORIENTED_EDGE('',*,*,#8718,.F.);
#12350=ORIENTED_EDGE('',*,*,#8884,.T.);
#12351=ORIENTED_EDGE('',*,*,#8756,.F.);
#12352=ORIENTED_EDGE('',*,*,#8885,.T.);
#12353=ORIENTED_EDGE('',*,*,#8719,.T.);
#12354=ORIENTED_EDGE('',*,*,#8885,.F.);
#12355=ORIENTED_EDGE('',*,*,#8755,.F.);
#12356=ORIENTED_EDGE('',*,*,#8886,.F.);
#12357=ORIENTED_EDGE('',*,*,#8720,.F.);
#12358=ORIENTED_EDGE('',*,*,#8886,.T.);
#12359=ORIENTED_EDGE('',*,*,#8754,.F.);
#12360=ORIENTED_EDGE('',*,*,#8887,.T.);
#12361=ORIENTED_EDGE('',*,*,#8721,.T.);
#12362=ORIENTED_EDGE('',*,*,#8887,.F.);
#12363=ORIENTED_EDGE('',*,*,#8753,.F.);
#12364=ORIENTED_EDGE('',*,*,#8888,.F.);
#12365=ORIENTED_EDGE('',*,*,#8722,.F.);
#12366=ORIENTED_EDGE('',*,*,#8888,.T.);
#12367=ORIENTED_EDGE('',*,*,#8752,.F.);
#12368=ORIENTED_EDGE('',*,*,#8889,.T.);
#12369=ORIENTED_EDGE('',*,*,#8723,.T.);
#12370=ORIENTED_EDGE('',*,*,#8889,.F.);
#12371=ORIENTED_EDGE('',*,*,#8751,.F.);
#12372=ORIENTED_EDGE('',*,*,#8890,.F.);
#12373=ORIENTED_EDGE('',*,*,#8724,.F.);
#12374=ORIENTED_EDGE('',*,*,#8890,.T.);
#12375=ORIENTED_EDGE('',*,*,#8750,.F.);
#12376=ORIENTED_EDGE('',*,*,#8891,.T.);
#12377=ORIENTED_EDGE('',*,*,#8725,.T.);
#12378=ORIENTED_EDGE('',*,*,#8891,.F.);
#12379=ORIENTED_EDGE('',*,*,#8749,.F.);
#12380=ORIENTED_EDGE('',*,*,#8892,.F.);
#12381=ORIENTED_EDGE('',*,*,#8726,.F.);
#12382=ORIENTED_EDGE('',*,*,#8892,.T.);
#12383=ORIENTED_EDGE('',*,*,#8748,.F.);
#12384=ORIENTED_EDGE('',*,*,#8893,.T.);
#12385=ORIENTED_EDGE('',*,*,#8727,.T.);
#12386=ORIENTED_EDGE('',*,*,#8893,.F.);
#12387=ORIENTED_EDGE('',*,*,#8747,.F.);
#12388=ORIENTED_EDGE('',*,*,#8894,.F.);
#12389=ORIENTED_EDGE('',*,*,#8728,.F.);
#12390=ORIENTED_EDGE('',*,*,#8894,.T.);
#12391=ORIENTED_EDGE('',*,*,#8746,.F.);
#12392=ORIENTED_EDGE('',*,*,#8895,.T.);
#12393=ORIENTED_EDGE('',*,*,#8729,.T.);
#12394=ORIENTED_EDGE('',*,*,#8895,.F.);
#12395=ORIENTED_EDGE('',*,*,#8745,.F.);
#12396=ORIENTED_EDGE('',*,*,#8896,.F.);
#12397=ORIENTED_EDGE('',*,*,#8730,.F.);
#12398=ORIENTED_EDGE('',*,*,#8896,.T.);
#12399=ORIENTED_EDGE('',*,*,#8744,.F.);
#12400=ORIENTED_EDGE('',*,*,#8897,.T.);
#12401=ORIENTED_EDGE('',*,*,#8731,.T.);
#12402=ORIENTED_EDGE('',*,*,#8898,.F.);
#12403=ORIENTED_EDGE('',*,*,#8732,.F.);
#12404=ORIENTED_EDGE('',*,*,#8897,.F.);
#12405=ORIENTED_EDGE('',*,*,#8743,.F.);
#12406=ORIENTED_EDGE('',*,*,#8821,.T.);
#12407=ORIENTED_EDGE('',*,*,#8735,.T.);
#12408=ORIENTED_EDGE('',*,*,#8899,.T.);
#12409=ORIENTED_EDGE('',*,*,#8740,.F.);
#12410=ORIENTED_EDGE('',*,*,#8900,.F.);
#12411=ORIENTED_EDGE('',*,*,#8741,.F.);
#12412=ORIENTED_EDGE('',*,*,#8899,.F.);
#12413=ORIENTED_EDGE('',*,*,#8734,.F.);
#12414=ORIENTED_EDGE('',*,*,#8898,.T.);
#12415=ORIENTED_EDGE('',*,*,#8742,.F.);
#12416=ORIENTED_EDGE('',*,*,#8900,.T.);
#12417=ORIENTED_EDGE('',*,*,#8733,.T.);
#12418=ORIENTED_EDGE('',*,*,#8901,.F.);
#12419=ORIENTED_EDGE('',*,*,#8902,.F.);
#12420=ORIENTED_EDGE('',*,*,#8903,.T.);
#12421=ORIENTED_EDGE('',*,*,#8901,.T.);
#12422=ORIENTED_EDGE('',*,*,#8903,.F.);
#12423=ORIENTED_EDGE('',*,*,#8904,.F.);
#12424=ORIENTED_EDGE('',*,*,#8905,.T.);
#12425=ORIENTED_EDGE('',*,*,#8902,.T.);
#12426=ORIENTED_EDGE('',*,*,#8905,.F.);
#12427=ORIENTED_EDGE('',*,*,#8906,.F.);
#12428=ORIENTED_EDGE('',*,*,#8907,.T.);
#12429=ORIENTED_EDGE('',*,*,#8904,.T.);
#12430=ORIENTED_EDGE('',*,*,#8907,.F.);
#12431=ORIENTED_EDGE('',*,*,#8906,.T.);
#12432=ORIENTED_EDGE('',*,*,#8908,.F.);
#12433=ORIENTED_EDGE('',*,*,#8909,.F.);
#12434=ORIENTED_EDGE('',*,*,#8910,.T.);
#12435=ORIENTED_EDGE('',*,*,#8908,.T.);
#12436=ORIENTED_EDGE('',*,*,#8910,.F.);
#12437=ORIENTED_EDGE('',*,*,#8911,.F.);
#12438=ORIENTED_EDGE('',*,*,#8912,.T.);
#12439=ORIENTED_EDGE('',*,*,#8909,.T.);
#12440=ORIENTED_EDGE('',*,*,#8912,.F.);
#12441=ORIENTED_EDGE('',*,*,#8913,.F.);
#12442=ORIENTED_EDGE('',*,*,#8914,.T.);
#12443=ORIENTED_EDGE('',*,*,#8911,.T.);
#12444=ORIENTED_EDGE('',*,*,#8914,.F.);
#12445=ORIENTED_EDGE('',*,*,#8913,.T.);
#12446=ORIENTED_EDGE('',*,*,#8915,.T.);
#12447=ORIENTED_EDGE('',*,*,#8916,.T.);
#12448=ORIENTED_EDGE('',*,*,#8917,.T.);
#12449=ORIENTED_EDGE('',*,*,#8918,.F.);
#12450=ORIENTED_EDGE('',*,*,#8919,.T.);
#12451=ORIENTED_EDGE('',*,*,#8920,.T.);
#12452=ORIENTED_EDGE('',*,*,#8921,.T.);
#12453=ORIENTED_EDGE('',*,*,#8916,.F.);
#12454=ORIENTED_EDGE('',*,*,#8922,.T.);
#12455=ORIENTED_EDGE('',*,*,#8923,.T.);
#12456=ORIENTED_EDGE('',*,*,#8924,.T.);
#12457=ORIENTED_EDGE('',*,*,#8920,.F.);
#12458=ORIENTED_EDGE('',*,*,#8925,.T.);
#12459=ORIENTED_EDGE('',*,*,#8926,.T.);
#12460=ORIENTED_EDGE('',*,*,#8927,.T.);
#12461=ORIENTED_EDGE('',*,*,#8923,.F.);
#12462=ORIENTED_EDGE('',*,*,#8928,.T.);
#12463=ORIENTED_EDGE('',*,*,#8929,.T.);
#12464=ORIENTED_EDGE('',*,*,#8930,.T.);
#12465=ORIENTED_EDGE('',*,*,#8926,.F.);
#12466=ORIENTED_EDGE('',*,*,#8931,.T.);
#12467=ORIENTED_EDGE('',*,*,#8918,.T.);
#12468=ORIENTED_EDGE('',*,*,#8932,.T.);
#12469=ORIENTED_EDGE('',*,*,#8929,.F.);
#12470=ORIENTED_EDGE('',*,*,#8931,.F.);
#12471=ORIENTED_EDGE('',*,*,#8928,.F.);
#12472=ORIENTED_EDGE('',*,*,#8925,.F.);
#12473=ORIENTED_EDGE('',*,*,#8922,.F.);
#12474=ORIENTED_EDGE('',*,*,#8919,.F.);
#12475=ORIENTED_EDGE('',*,*,#8915,.F.);
#12476=ORIENTED_EDGE('',*,*,#8932,.F.);
#12477=ORIENTED_EDGE('',*,*,#8917,.F.);
#12478=ORIENTED_EDGE('',*,*,#8921,.F.);
#12479=ORIENTED_EDGE('',*,*,#8924,.F.);
#12480=ORIENTED_EDGE('',*,*,#8927,.F.);
#12481=ORIENTED_EDGE('',*,*,#8930,.F.);
#12482=ORIENTED_EDGE('',*,*,#8933,.F.);
#12483=ORIENTED_EDGE('',*,*,#8934,.T.);
#12484=ORIENTED_EDGE('',*,*,#8935,.T.);
#12485=ORIENTED_EDGE('',*,*,#8936,.F.);
#12486=ORIENTED_EDGE('',*,*,#8937,.F.);
#12487=ORIENTED_EDGE('',*,*,#8938,.T.);
#12488=ORIENTED_EDGE('',*,*,#8939,.T.);
#12489=ORIENTED_EDGE('',*,*,#8934,.F.);
#12490=ORIENTED_EDGE('',*,*,#8940,.F.);
#12491=ORIENTED_EDGE('',*,*,#8941,.T.);
#12492=ORIENTED_EDGE('',*,*,#8942,.T.);
#12493=ORIENTED_EDGE('',*,*,#8938,.F.);
#12494=ORIENTED_EDGE('',*,*,#8943,.F.);
#12495=ORIENTED_EDGE('',*,*,#8944,.T.);
#12496=ORIENTED_EDGE('',*,*,#8945,.T.);
#12497=ORIENTED_EDGE('',*,*,#8941,.F.);
#12498=ORIENTED_EDGE('',*,*,#8946,.F.);
#12499=ORIENTED_EDGE('',*,*,#8947,.T.);
#12500=ORIENTED_EDGE('',*,*,#8948,.T.);
#12501=ORIENTED_EDGE('',*,*,#8944,.F.);
#12502=ORIENTED_EDGE('',*,*,#8949,.F.);
#12503=ORIENTED_EDGE('',*,*,#8936,.T.);
#12504=ORIENTED_EDGE('',*,*,#8950,.T.);
#12505=ORIENTED_EDGE('',*,*,#8947,.F.);
#12506=ORIENTED_EDGE('',*,*,#8950,.F.);
#12507=ORIENTED_EDGE('',*,*,#8935,.F.);
#12508=ORIENTED_EDGE('',*,*,#8939,.F.);
#12509=ORIENTED_EDGE('',*,*,#8942,.F.);
#12510=ORIENTED_EDGE('',*,*,#8945,.F.);
#12511=ORIENTED_EDGE('',*,*,#8948,.F.);
#12512=ORIENTED_EDGE('',*,*,#8951,.F.);
#12513=ORIENTED_EDGE('',*,*,#8933,.T.);
#12514=ORIENTED_EDGE('',*,*,#8949,.T.);
#12515=ORIENTED_EDGE('',*,*,#8946,.T.);
#12516=ORIENTED_EDGE('',*,*,#8943,.T.);
#12517=ORIENTED_EDGE('',*,*,#8940,.T.);
#12518=ORIENTED_EDGE('',*,*,#8937,.T.);
#12519=ORIENTED_EDGE('',*,*,#8952,.F.);
#12520=ORIENTED_EDGE('',*,*,#8953,.T.);
#12521=ORIENTED_EDGE('',*,*,#8951,.T.);
#12522=ORIENTED_EDGE('',*,*,#8953,.F.);
#12523=ORIENTED_EDGE('',*,*,#8954,.F.);
#12524=ORIENTED_EDGE('',*,*,#8955,.T.);
#12525=ORIENTED_EDGE('',*,*,#8952,.T.);
#12526=ORIENTED_EDGE('',*,*,#8955,.F.);
#12527=ORIENTED_EDGE('',*,*,#8956,.F.);
#12528=ORIENTED_EDGE('',*,*,#8957,.T.);
#12529=ORIENTED_EDGE('',*,*,#8954,.T.);
#12530=ORIENTED_EDGE('',*,*,#8957,.F.);
#12531=ORIENTED_EDGE('',*,*,#8956,.T.);
#12532=CYLINDRICAL_SURFACE('',#14565,0.165);
#12533=CYLINDRICAL_SURFACE('',#14569,0.165);
#12534=CYLINDRICAL_SURFACE('',#14573,0.210000000000001);
#12535=CYLINDRICAL_SURFACE('',#14577,0.210000000000001);
#12536=CYLINDRICAL_SURFACE('',#14581,0.21);
#12537=CYLINDRICAL_SURFACE('',#14585,0.21);
#12538=CYLINDRICAL_SURFACE('',#14589,0.210000000000001);
#12539=CYLINDRICAL_SURFACE('',#14593,0.210000000000001);
#12540=CYLINDRICAL_SURFACE('',#14597,0.21);
#12541=CYLINDRICAL_SURFACE('',#14601,0.21);
#12542=CYLINDRICAL_SURFACE('',#14605,0.225);
#12543=CYLINDRICAL_SURFACE('',#14608,0.225);
#12544=CYLINDRICAL_SURFACE('',#14620,0.225);
#12545=CYLINDRICAL_SURFACE('',#14622,0.225);
#12546=CYLINDRICAL_SURFACE('',#14626,0.225);
#12547=CYLINDRICAL_SURFACE('',#14630,0.225);
#12548=CYLINDRICAL_SURFACE('',#14634,0.225);
#12549=CYLINDRICAL_SURFACE('',#14638,0.225);
#12550=CYLINDRICAL_SURFACE('',#14642,0.165);
#12551=CYLINDRICAL_SURFACE('',#14646,0.165);
#12552=CYLINDRICAL_SURFACE('',#14650,0.165);
#12553=CYLINDRICAL_SURFACE('',#14654,0.165);
#12554=CYLINDRICAL_SURFACE('',#14678,0.165);
#12555=CYLINDRICAL_SURFACE('',#14681,0.165);
#12556=CYLINDRICAL_SURFACE('',#14684,0.165);
#12557=CYLINDRICAL_SURFACE('',#14687,0.165);
#12558=CYLINDRICAL_SURFACE('',#14690,1.5);
#12559=CYLINDRICAL_SURFACE('',#14693,0.225);
#12560=CYLINDRICAL_SURFACE('',#14696,0.225);
#12561=CYLINDRICAL_SURFACE('',#14699,0.225);
#12562=CYLINDRICAL_SURFACE('',#14702,0.225);
#12563=CYLINDRICAL_SURFACE('',#14716,1.1);
#12564=CYLINDRICAL_SURFACE('',#14719,1.49);
#12565=CYLINDRICAL_SURFACE('',#14725,0.225);
#12566=CYLINDRICAL_SURFACE('',#14728,0.225);
#12567=CYLINDRICAL_SURFACE('',#14731,0.225);
#12568=CYLINDRICAL_SURFACE('',#14734,0.225);
#12569=CYLINDRICAL_SURFACE('',#14743,2.1);
#12570=CYLINDRICAL_SURFACE('',#14745,2.1);
#12571=CYLINDRICAL_SURFACE('',#14747,2.1);
#12572=CYLINDRICAL_SURFACE('',#14749,2.1);
#12573=CYLINDRICAL_SURFACE('',#14751,1.49);
#12574=CYLINDRICAL_SURFACE('',#14756,1.1);
#12575=CYLINDRICAL_SURFACE('',#14759,0.225);
#12576=CYLINDRICAL_SURFACE('',#14762,0.225);
#12577=CYLINDRICAL_SURFACE('',#14765,0.225);
#12578=CYLINDRICAL_SURFACE('',#14768,0.225);
#12579=CYLINDRICAL_SURFACE('',#14777,2.1);
#12580=CYLINDRICAL_SURFACE('',#14779,2.1);
#12581=CYLINDRICAL_SURFACE('',#14781,2.1);
#12582=CYLINDRICAL_SURFACE('',#14783,2.1);
#12583=CYLINDRICAL_SURFACE('',#14785,1.49);
#12584=CYLINDRICAL_SURFACE('',#14789,1.1);
#12585=CYLINDRICAL_SURFACE('',#14793,2.21);
#12586=CYLINDRICAL_SURFACE('',#14796,2.21);
#12587=CYLINDRICAL_SURFACE('',#14806,2.21);
#12588=CYLINDRICAL_SURFACE('',#14812,0.165);
#12589=CYLINDRICAL_SURFACE('',#14814,0.165);
#12590=CYLINDRICAL_SURFACE('',#14816,0.164999999999999);
#12591=CYLINDRICAL_SURFACE('',#14818,0.164999999999999);
#12592=CYLINDRICAL_SURFACE('',#14820,1.6);
#12593=CYLINDRICAL_SURFACE('',#14822,0.225);
#12594=CYLINDRICAL_SURFACE('',#14825,0.225);
#12595=CYLINDRICAL_SURFACE('',#14828,0.225);
#12596=CYLINDRICAL_SURFACE('',#14831,0.225);
#12597=CYLINDRICAL_SURFACE('',#14843,0.165);
#12598=CYLINDRICAL_SURFACE('',#14846,0.4);
#12599=CYLINDRICAL_SURFACE('',#14852,0.165);
#12600=CYLINDRICAL_SURFACE('',#14855,0.4);
#12601=CYLINDRICAL_SURFACE('',#14861,0.164999999999999);
#12602=CYLINDRICAL_SURFACE('',#14864,0.4);
#12603=CYLINDRICAL_SURFACE('',#14870,0.164999999999999);
#12604=CYLINDRICAL_SURFACE('',#14873,0.4);
#12605=CYLINDRICAL_SURFACE('',#14879,1.2);
#12606=CYLINDRICAL_SURFACE('',#14882,1.59);
#12607=CYLINDRICAL_SURFACE('',#14888,0.225);
#12608=CYLINDRICAL_SURFACE('',#14891,0.225);
#12609=CYLINDRICAL_SURFACE('',#14894,0.225);
#12610=CYLINDRICAL_SURFACE('',#14897,0.225);
#12611=CYLINDRICAL_SURFACE('',#14906,2.2);
#12612=CYLINDRICAL_SURFACE('',#14908,2.2);
#12613=CYLINDRICAL_SURFACE('',#14910,2.2);
#12614=CYLINDRICAL_SURFACE('',#14912,2.2);
#12615=CYLINDRICAL_SURFACE('',#14914,1.59);
#12616=CYLINDRICAL_SURFACE('',#14919,1.2);
#12617=CYLINDRICAL_SURFACE('',#14922,0.375);
#12618=CYLINDRICAL_SURFACE('',#14934,0.375);
#12619=CYLINDRICAL_SURFACE('',#14941,0.375);
#12620=CYLINDRICAL_SURFACE('',#14948,0.375);
#12621=CYLINDRICAL_SURFACE('',#14950,0.225);
#12622=CYLINDRICAL_SURFACE('',#14952,0.225);
#12623=CYLINDRICAL_SURFACE('',#14954,0.225);
#12624=CYLINDRICAL_SURFACE('',#14956,2.2);
#12625=CYLINDRICAL_SURFACE('',#14970,2.2);
#12626=CYLINDRICAL_SURFACE('',#14971,2.2);
#12627=CYLINDRICAL_SURFACE('',#14972,0.225);
#12628=CYLINDRICAL_SURFACE('',#14973,2.2);
#12629=CYLINDRICAL_SURFACE('',#14974,1.2);
#12630=CYLINDRICAL_SURFACE('',#14983,0.636619772367581);
#12631=CYLINDRICAL_SURFACE('',#14985,1.27323954473516);
#12632=CYLINDRICAL_SURFACE('',#14987,1.37323954473516);
#12633=CYLINDRICAL_SURFACE('',#14991,0.736619772367581);
#12634=CYLINDRICAL_SURFACE('',#14995,0.475);
#12635=CYLINDRICAL_SURFACE('',#15000,0.275);
#12636=CYLINDRICAL_SURFACE('',#15002,0.475);
#12637=CYLINDRICAL_SURFACE('',#15007,0.275);
#12638=CYLINDRICAL_SURFACE('',#15009,0.475);
#12639=CYLINDRICAL_SURFACE('',#15014,0.275);
#12640=CYLINDRICAL_SURFACE('',#15016,0.475);
#12641=CYLINDRICAL_SURFACE('',#15021,0.275);
#12642=CYLINDRICAL_SURFACE('',#15023,0.34);
#12643=CYLINDRICAL_SURFACE('',#15027,0.34);
#12644=CYLINDRICAL_SURFACE('',#15038,0.425);
#12645=CYLINDRICAL_SURFACE('',#15041,0.645);
#12646=CYLINDRICAL_SURFACE('',#15047,0.425000000000001);
#12647=CYLINDRICAL_SURFACE('',#15050,0.645);
#12648=CYLINDRICAL_SURFACE('',#15056,0.475);
#12649=CYLINDRICAL_SURFACE('',#15061,0.275);
#12650=CYLINDRICAL_SURFACE('',#15063,0.475);
#12651=CYLINDRICAL_SURFACE('',#15068,0.275);
#12652=CYLINDRICAL_SURFACE('',#15070,0.475);
#12653=CYLINDRICAL_SURFACE('',#15075,0.275);
#12654=CYLINDRICAL_SURFACE('',#15077,0.475);
#12655=CYLINDRICAL_SURFACE('',#15082,0.275);
#12656=CYLINDRICAL_SURFACE('',#15084,0.34);
#12657=CYLINDRICAL_SURFACE('',#15088,0.34);
#12658=CYLINDRICAL_SURFACE('',#15099,0.425);
#12659=CYLINDRICAL_SURFACE('',#15102,0.645);
#12660=CYLINDRICAL_SURFACE('',#15108,0.425000000000001);
#12661=CYLINDRICAL_SURFACE('',#15111,0.645);
#12662=CYLINDRICAL_SURFACE('',#15117,0.4);
#12663=CYLINDRICAL_SURFACE('',#15122,0.225);
#12664=CYLINDRICAL_SURFACE('',#15124,0.4);
#12665=CYLINDRICAL_SURFACE('',#15129,0.225);
#12666=CYLINDRICAL_SURFACE('',#15145,0.165);
#12667=CYLINDRICAL_SURFACE('',#15148,0.165);
#12668=CYLINDRICAL_SURFACE('',#15158,0.164999999999999);
#12669=CYLINDRICAL_SURFACE('',#15161,0.164999999999999);
#12670=CYLINDRICAL_SURFACE('',#15171,0.225);
#12671=CYLINDRICAL_SURFACE('',#15174,0.225);
#12672=CYLINDRICAL_SURFACE('',#15177,0.225);
#12673=CYLINDRICAL_SURFACE('',#15180,0.225);
#12674=CYLINDRICAL_SURFACE('',#15197,0.976185);
#12675=CYLINDRICAL_SURFACE('',#15199,0.5);
#12676=CYLINDRICAL_SURFACE('',#15205,0.976185);
#12677=CYLINDRICAL_SURFACE('',#15217,1.023815);
#12678=CYLINDRICAL_SURFACE('',#15224,1.5);
#12679=CYLINDRICAL_SURFACE('',#15229,1.023815);
#12680=CYLINDRICAL_SURFACE('',#15251,1.019052);
#12681=CYLINDRICAL_SURFACE('',#15291,0.980948);
#12682=CYLINDRICAL_SURFACE('',#15305,1.013815);
#12683=CYLINDRICAL_SURFACE('',#15309,0.991185);
#12684=CYLINDRICAL_SURFACE('',#15313,1.013815);
#12685=CYLINDRICAL_SURFACE('',#15317,0.991185);
#12686=CYLINDRICAL_SURFACE('',#15335,0.2);
#12687=CYLINDRICAL_SURFACE('',#15342,0.35);
#12688=CYLINDRICAL_SURFACE('',#15350,0.1954);
#12689=CYLINDRICAL_SURFACE('',#15361,1.070235);
#12690=CYLINDRICAL_SURFACE('',#15363,0.6);
#12691=CYLINDRICAL_SURFACE('',#15369,1.070235);
#12692=CYLINDRICAL_SURFACE('',#15381,1.129765);
#12693=CYLINDRICAL_SURFACE('',#15388,1.6);
#12694=CYLINDRICAL_SURFACE('',#15393,1.129765);
#12695=CYLINDRICAL_SURFACE('',#15413,1.123812);
#12696=CYLINDRICAL_SURFACE('',#15449,1.076188);
#12697=CYLINDRICAL_SURFACE('',#15463,1.119765);
#12698=CYLINDRICAL_SURFACE('',#15467,1.085235);
#12699=CYLINDRICAL_SURFACE('',#15471,1.119765);
#12700=CYLINDRICAL_SURFACE('',#15475,1.085235);
#12701=CYLINDRICAL_SURFACE('',#15486,0.425);
#12702=CYLINDRICAL_SURFACE('',#15494,0.24505);
#12703=CYLINDRICAL_SURFACE('',#15509,2.05);
#12704=CYLINDRICAL_SURFACE('',#15512,2.05);
#12705=CYLINDRICAL_SURFACE('',#15530,2.8);
#12706=CYLINDRICAL_SURFACE('',#15540,0.65);
#12707=CYLINDRICAL_SURFACE('',#15542,0.65);
#12708=CYLINDRICAL_SURFACE('',#15550,1.8);
#12709=CYLINDRICAL_SURFACE('',#15559,0.25);
#12710=CYLINDRICAL_SURFACE('',#15560,0.25);
#12711=CYLINDRICAL_SURFACE('',#15561,1.65);
#12712=CYLINDRICAL_SURFACE('',#15564,0.25);
#12713=CYLINDRICAL_SURFACE('',#15565,0.25);
#12714=CYLINDRICAL_SURFACE('',#15566,0.25);
#12715=CYLINDRICAL_SURFACE('',#15567,0.25);
#12716=CYLINDRICAL_SURFACE('',#15572,1.75);
#12717=CYLINDRICAL_SURFACE('',#15576,1.);
#12718=CYLINDRICAL_SURFACE('',#15580,0.42);
#12719=CYLINDRICAL_SURFACE('',#15583,0.8);
#12720=CYLINDRICAL_SURFACE('',#15603,0.65);
#12721=CYLINDRICAL_SURFACE('',#15611,0.3933);
#12722=CYLINDRICAL_SURFACE('',#15627,0.35);
#12723=CYLINDRICAL_SURFACE('',#15635,0.1954);
#12724=CYLINDRICAL_SURFACE('',#15638,0.165);
#12725=CYLINDRICAL_SURFACE('',#15648,0.7);
#12726=CYLINDRICAL_SURFACE('',#15649,0.5);
#12727=CYLINDRICAL_SURFACE('',#15651,0.4);
#12728=CYLINDRICAL_SURFACE('',#15655,0.5);
#12729=CYLINDRICAL_SURFACE('',#15660,0.505);
#12730=CYLINDRICAL_SURFACE('',#15665,0.405);
#12731=CYLINDRICAL_SURFACE('',#15667,0.7);
#12732=CYLINDRICAL_SURFACE('',#15673,0.505);
#12733=CYLINDRICAL_SURFACE('',#15676,0.7);
#12734=CYLINDRICAL_SURFACE('',#15682,0.15);
#12735=CYLINDRICAL_SURFACE('',#15688,0.15);
#12736=CYLINDRICAL_SURFACE('',#15694,0.225);
#12737=CYLINDRICAL_SURFACE('',#15697,0.6);
#12738=CYLINDRICAL_SURFACE('',#15703,0.5);
#12739=CYLINDRICAL_SURFACE('',#15711,0.21);
#12740=CYLINDRICAL_SURFACE('',#15717,0.21);
#12741=CYLINDRICAL_SURFACE('',#15721,0.505);
#12742=CYLINDRICAL_SURFACE('',#15724,1.);
#12743=CYLINDRICAL_SURFACE('',#15730,0.125);
#12744=CYLINDRICAL_SURFACE('',#15731,0.125);
#12745=CYLINDRICAL_SURFACE('',#15732,0.65);
#12746=CYLINDRICAL_SURFACE('',#15735,0.125);
#12747=CYLINDRICAL_SURFACE('',#15736,0.125);
#12748=CYLINDRICAL_SURFACE('',#15737,0.4);
#12749=CYLINDRICAL_SURFACE('',#15783,0.8);
#12750=CYLINDRICAL_SURFACE('',#15828,0.8);
#12751=CYLINDRICAL_SURFACE('',#15831,0.0555);
#12752=CYLINDRICAL_SURFACE('',#15832,0.611219772367581);
#12753=CYLINDRICAL_SURFACE('',#15833,0.0555);
#12754=CYLINDRICAL_SURFACE('',#15834,0.611219772367581);
#12755=CYLINDRICAL_SURFACE('',#15835,0.0555);
#12756=CYLINDRICAL_SURFACE('',#15836,0.611219772367581);
#12757=CYLINDRICAL_SURFACE('',#15837,0.0555);
#12758=CYLINDRICAL_SURFACE('',#15838,0.611219772367581);
#12759=CYLINDRICAL_SURFACE('',#15839,0.0555);
#12760=CYLINDRICAL_SURFACE('',#15840,0.611219772367581);
#12761=CYLINDRICAL_SURFACE('',#15841,0.0555);
#12762=CYLINDRICAL_SURFACE('',#15842,0.611219772367581);
#12763=CYLINDRICAL_SURFACE('',#15843,0.0555);
#12764=CYLINDRICAL_SURFACE('',#15844,0.611219772367581);
#12765=CYLINDRICAL_SURFACE('',#15845,0.0555);
#12766=CYLINDRICAL_SURFACE('',#15846,0.611219772367581);
#12767=CYLINDRICAL_SURFACE('',#15847,0.0555);
#12768=CYLINDRICAL_SURFACE('',#15848,0.611219772367581);
#12769=CYLINDRICAL_SURFACE('',#15849,0.0555);
#12770=CYLINDRICAL_SURFACE('',#15850,0.611219772367581);
#12771=CYLINDRICAL_SURFACE('',#15851,0.0555);
#12772=CYLINDRICAL_SURFACE('',#15852,0.611219772367581);
#12773=CYLINDRICAL_SURFACE('',#15853,0.0555);
#12774=CYLINDRICAL_SURFACE('',#15854,0.611219772367581);
#12775=CYLINDRICAL_SURFACE('',#15855,0.0555);
#12776=CYLINDRICAL_SURFACE('',#15856,0.611219772367581);
#12777=CYLINDRICAL_SURFACE('',#15857,0.0555);
#12778=CYLINDRICAL_SURFACE('',#15858,0.611219772367581);
#12779=CYLINDRICAL_SURFACE('',#15859,0.0555);
#12780=CYLINDRICAL_SURFACE('',#15860,0.611219772367581);
#12781=CYLINDRICAL_SURFACE('',#15861,0.0555);
#12782=CYLINDRICAL_SURFACE('',#15862,0.611219772367581);
#12783=CYLINDRICAL_SURFACE('',#15863,0.0555);
#12784=CYLINDRICAL_SURFACE('',#15864,0.611219772367581);
#12785=CYLINDRICAL_SURFACE('',#15865,0.0555);
#12786=CYLINDRICAL_SURFACE('',#15866,0.611219772367581);
#12787=CYLINDRICAL_SURFACE('',#15867,0.0555);
#12788=CYLINDRICAL_SURFACE('',#15868,0.611219772367581);
#12789=CYLINDRICAL_SURFACE('',#15869,0.0555);
#12790=CYLINDRICAL_SURFACE('',#15870,0.611219772367581);
#12791=CYLINDRICAL_SURFACE('',#15876,1.);
#12792=CYLINDRICAL_SURFACE('',#15879,0.165);
#12793=CYLINDRICAL_SURFACE('',#15886,0.8);
#12794=CYLINDRICAL_SURFACE('',#15887,0.6);
#12795=CYLINDRICAL_SURFACE('',#15891,0.605);
#12796=CYLINDRICAL_SURFACE('',#15894,0.8);
#12797=CYLINDRICAL_SURFACE('',#15900,0.605);
#12798=CYLINDRICAL_SURFACE('',#15903,0.8);
#12799=CYLINDRICAL_SURFACE('',#15909,0.15);
#12800=CYLINDRICAL_SURFACE('',#15915,0.15);
#12801=CYLINDRICAL_SURFACE('',#15921,0.225);
#12802=CYLINDRICAL_SURFACE('',#15924,0.8);
#12803=CYLINDRICAL_SURFACE('',#15932,0.21);
#12804=CYLINDRICAL_SURFACE('',#15936,1.005);
#12805=CYLINDRICAL_SURFACE('',#15939,1.5);
#12806=CYLINDRICAL_SURFACE('',#15947,0.21);
#12807=CYLINDRICAL_SURFACE('',#15951,1.005);
#12808=CYLINDRICAL_SURFACE('',#15954,1.5);
#12809=CYLINDRICAL_SURFACE('',#15960,3.6);
#12810=CYLINDRICAL_SURFACE('',#15963,4.);
#12811=CYLINDRICAL_SURFACE('',#15969,1.005);
#12812=CYLINDRICAL_SURFACE('',#15972,4.);
#12813=CYLINDRICAL_SURFACE('',#15978,1.005);
#12814=CYLINDRICAL_SURFACE('',#15981,4.);
#12815=CYLINDRICAL_SURFACE('',#15989,0.21);
#12816=CYLINDRICAL_SURFACE('',#15993,1.005);
#12817=CYLINDRICAL_SURFACE('',#15996,1.8);
#12818=CYLINDRICAL_SURFACE('',#16004,0.21);
#12819=CYLINDRICAL_SURFACE('',#16008,1.005);
#12820=CYLINDRICAL_SURFACE('',#16011,1.8);
#12821=CYLINDRICAL_SURFACE('',#16017,0.125);
#12822=CYLINDRICAL_SURFACE('',#16018,0.125);
#12823=CYLINDRICAL_SURFACE('',#16019,1.);
#12824=CYLINDRICAL_SURFACE('',#16022,0.125);
#12825=CYLINDRICAL_SURFACE('',#16023,0.125);
#12826=CYLINDRICAL_SURFACE('',#16024,0.6);
#12827=CYLINDRICAL_SURFACE('',#16110,1.4);
#12828=CYLINDRICAL_SURFACE('',#16195,1.4);
#12829=CYLINDRICAL_SURFACE('',#16198,0.0555000000000001);
#12830=CYLINDRICAL_SURFACE('',#16199,1.24783954473516);
#12831=CYLINDRICAL_SURFACE('',#16200,0.0555000000000001);
#12832=CYLINDRICAL_SURFACE('',#16201,1.24783954473516);
#12833=CYLINDRICAL_SURFACE('',#16202,0.0555000000000001);
#12834=CYLINDRICAL_SURFACE('',#16203,1.24783954473516);
#12835=CYLINDRICAL_SURFACE('',#16204,0.0555000000000001);
#12836=CYLINDRICAL_SURFACE('',#16205,1.24783954473516);
#12837=CYLINDRICAL_SURFACE('',#16206,0.0555000000000001);
#12838=CYLINDRICAL_SURFACE('',#16207,1.24783954473516);
#12839=CYLINDRICAL_SURFACE('',#16208,0.0555000000000001);
#12840=CYLINDRICAL_SURFACE('',#16209,1.24783954473516);
#12841=CYLINDRICAL_SURFACE('',#16210,0.0555000000000001);
#12842=CYLINDRICAL_SURFACE('',#16211,1.24783954473516);
#12843=CYLINDRICAL_SURFACE('',#16212,0.0555000000000001);
#12844=CYLINDRICAL_SURFACE('',#16213,1.24783954473516);
#12845=CYLINDRICAL_SURFACE('',#16214,0.0555000000000001);
#12846=CYLINDRICAL_SURFACE('',#16215,1.24783954473516);
#12847=CYLINDRICAL_SURFACE('',#16216,0.0555000000000001);
#12848=CYLINDRICAL_SURFACE('',#16217,1.24783954473516);
#12849=CYLINDRICAL_SURFACE('',#16218,0.0555000000000001);
#12850=CYLINDRICAL_SURFACE('',#16219,1.24783954473516);
#12851=CYLINDRICAL_SURFACE('',#16220,0.0555000000000001);
#12852=CYLINDRICAL_SURFACE('',#16221,1.24783954473516);
#12853=CYLINDRICAL_SURFACE('',#16222,0.0555000000000001);
#12854=CYLINDRICAL_SURFACE('',#16223,1.24783954473516);
#12855=CYLINDRICAL_SURFACE('',#16224,0.0555000000000001);
#12856=CYLINDRICAL_SURFACE('',#16225,1.24783954473516);
#12857=CYLINDRICAL_SURFACE('',#16226,0.0555000000000001);
#12858=CYLINDRICAL_SURFACE('',#16227,1.24783954473516);
#12859=CYLINDRICAL_SURFACE('',#16228,0.0555000000000001);
#12860=CYLINDRICAL_SURFACE('',#16229,1.24783954473516);
#12861=CYLINDRICAL_SURFACE('',#16230,0.0555000000000001);
#12862=CYLINDRICAL_SURFACE('',#16231,1.24783954473516);
#12863=CYLINDRICAL_SURFACE('',#16232,0.0555000000000001);
#12864=CYLINDRICAL_SURFACE('',#16233,1.24783954473516);
#12865=CYLINDRICAL_SURFACE('',#16234,0.0555000000000001);
#12866=CYLINDRICAL_SURFACE('',#16235,1.24783954473516);
#12867=CYLINDRICAL_SURFACE('',#16236,0.0555000000000001);
#12868=CYLINDRICAL_SURFACE('',#16237,1.24783954473516);
#12869=CYLINDRICAL_SURFACE('',#16238,0.0555000000000001);
#12870=CYLINDRICAL_SURFACE('',#16239,1.24783954473516);
#12871=CYLINDRICAL_SURFACE('',#16240,0.0555000000000001);
#12872=CYLINDRICAL_SURFACE('',#16241,1.24783954473516);
#12873=CYLINDRICAL_SURFACE('',#16242,0.0555000000000001);
#12874=CYLINDRICAL_SURFACE('',#16243,1.24783954473516);
#12875=CYLINDRICAL_SURFACE('',#16244,0.0555000000000001);
#12876=CYLINDRICAL_SURFACE('',#16245,1.24783954473516);
#12877=CYLINDRICAL_SURFACE('',#16246,0.0555000000000001);
#12878=CYLINDRICAL_SURFACE('',#16247,1.24783954473516);
#12879=CYLINDRICAL_SURFACE('',#16248,0.0555000000000001);
#12880=CYLINDRICAL_SURFACE('',#16249,1.24783954473516);
#12881=CYLINDRICAL_SURFACE('',#16250,0.0555000000000001);
#12882=CYLINDRICAL_SURFACE('',#16251,1.24783954473516);
#12883=CYLINDRICAL_SURFACE('',#16252,0.0555000000000001);
#12884=CYLINDRICAL_SURFACE('',#16253,1.24783954473516);
#12885=CYLINDRICAL_SURFACE('',#16254,0.0555000000000001);
#12886=CYLINDRICAL_SURFACE('',#16255,1.24783954473516);
#12887=CYLINDRICAL_SURFACE('',#16256,0.0555000000000001);
#12888=CYLINDRICAL_SURFACE('',#16257,1.24783954473516);
#12889=CYLINDRICAL_SURFACE('',#16258,0.0555000000000001);
#12890=CYLINDRICAL_SURFACE('',#16259,1.24783954473516);
#12891=CYLINDRICAL_SURFACE('',#16260,0.0555000000000001);
#12892=CYLINDRICAL_SURFACE('',#16261,1.24783954473516);
#12893=CYLINDRICAL_SURFACE('',#16262,0.0555000000000001);
#12894=CYLINDRICAL_SURFACE('',#16263,1.24783954473516);
#12895=CYLINDRICAL_SURFACE('',#16264,0.0555000000000001);
#12896=CYLINDRICAL_SURFACE('',#16265,1.24783954473516);
#12897=CYLINDRICAL_SURFACE('',#16266,0.0555000000000001);
#12898=CYLINDRICAL_SURFACE('',#16267,1.24783954473516);
#12899=CYLINDRICAL_SURFACE('',#16268,0.0555000000000001);
#12900=CYLINDRICAL_SURFACE('',#16269,1.24783954473516);
#12901=CYLINDRICAL_SURFACE('',#16270,0.0555000000000001);
#12902=CYLINDRICAL_SURFACE('',#16271,1.24783954473516);
#12903=CYLINDRICAL_SURFACE('',#16272,0.0555000000000001);
#12904=CYLINDRICAL_SURFACE('',#16273,1.24783954473516);
#12905=CYLINDRICAL_SURFACE('',#16274,0.0555000000000001);
#12906=CYLINDRICAL_SURFACE('',#16275,1.24783954473516);
#12907=CYLINDRICAL_SURFACE('',#16276,0.0555000000000001);
#12908=CYLINDRICAL_SURFACE('',#16277,1.24783954473516);
#12909=CYLINDRICAL_SURFACE('',#16283,0.35);
#12910=CYLINDRICAL_SURFACE('',#16291,0.1954);
#12911=CYLINDRICAL_SURFACE('',#16395,0.24505);
#12912=ADVANCED_FACE('',(#1633),#12532,.F.);
#12913=ADVANCED_FACE('',(#1634),#1277,.T.);
#12914=ADVANCED_FACE('',(#1635),#12533,.F.);
#12915=ADVANCED_FACE('',(#1636),#1278,.T.);
#12916=ADVANCED_FACE('',(#1637),#12534,.F.);
#12917=ADVANCED_FACE('',(#1638),#1279,.T.);
#12918=ADVANCED_FACE('',(#1639),#12535,.F.);
#12919=ADVANCED_FACE('',(#1640),#1280,.T.);
#12920=ADVANCED_FACE('',(#1641),#12536,.F.);
#12921=ADVANCED_FACE('',(#1642),#1281,.T.);
#12922=ADVANCED_FACE('',(#1643),#12537,.F.);
#12923=ADVANCED_FACE('',(#1644),#1282,.T.);
#12924=ADVANCED_FACE('',(#1645),#12538,.F.);
#12925=ADVANCED_FACE('',(#1646),#1283,.T.);
#12926=ADVANCED_FACE('',(#1647),#12539,.F.);
#12927=ADVANCED_FACE('',(#1648),#1284,.T.);
#12928=ADVANCED_FACE('',(#1649),#12540,.F.);
#12929=ADVANCED_FACE('',(#1650),#1285,.T.);
#12930=ADVANCED_FACE('',(#1651),#12541,.F.);
#12931=ADVANCED_FACE('',(#1652),#1286,.T.);
#12932=ADVANCED_FACE('',(#1653),#12542,.F.);
#12933=ADVANCED_FACE('',(#1654),#12543,.F.);
#12934=ADVANCED_FACE('',(#1655,#1012,#1013,#1014,#1015),#1287,.F.);
#12935=ADVANCED_FACE('',(#1656),#1288,.F.);
#12936=ADVANCED_FACE('',(#1657),#1289,.F.);
#12937=ADVANCED_FACE('',(#1658),#12544,.F.);
#12938=ADVANCED_FACE('',(#1659),#12545,.F.);
#12939=ADVANCED_FACE('',(#1660),#1290,.F.);
#12940=ADVANCED_FACE('',(#1661),#1291,.F.);
#12941=ADVANCED_FACE('',(#1662),#12546,.F.);
#12942=ADVANCED_FACE('',(#1663),#12547,.F.);
#12943=ADVANCED_FACE('',(#1664),#1292,.F.);
#12944=ADVANCED_FACE('',(#1665),#1293,.F.);
#12945=ADVANCED_FACE('',(#1666),#12548,.F.);
#12946=ADVANCED_FACE('',(#1667),#12549,.F.);
#12947=ADVANCED_FACE('',(#1668),#1294,.F.);
#12948=ADVANCED_FACE('',(#1669),#1295,.F.);
#12949=ADVANCED_FACE('',(#1670),#12550,.F.);
#12950=ADVANCED_FACE('',(#1671),#1296,.T.);
#12951=ADVANCED_FACE('',(#1672),#12551,.F.);
#12952=ADVANCED_FACE('',(#1673),#1297,.T.);
#12953=ADVANCED_FACE('',(#1674),#12552,.F.);
#12954=ADVANCED_FACE('',(#1675),#1298,.T.);
#12955=ADVANCED_FACE('',(#1676),#12553,.F.);
#12956=ADVANCED_FACE('',(#1677),#1299,.T.);
#12957=ADVANCED_FACE('',(#1678),#1300,.T.);
#12958=ADVANCED_FACE('',(#1679),#1301,.T.);
#12959=ADVANCED_FACE('',(#1680),#1302,.T.);
#12960=ADVANCED_FACE('',(#1681),#1303,.T.);
#12961=ADVANCED_FACE('',(#1682,#1016,#1017,#1018,#1019,#1020,#1021,#1022,
#1023,#1024,#1025,#1026,#1027,#1028,#1029,#1030,#1031),#1304,.T.);
#12962=ADVANCED_FACE('',(#1683),#1305,.T.);
#12963=ADVANCED_FACE('',(#1684),#1306,.T.);
#12964=ADVANCED_FACE('',(#1685),#1307,.T.);
#12965=ADVANCED_FACE('',(#1686),#1308,.T.);
#12966=ADVANCED_FACE('',(#1687),#1309,.T.);
#12967=ADVANCED_FACE('',(#1688),#1310,.F.);
#12968=ADVANCED_FACE('',(#1689),#1311,.T.);
#12969=ADVANCED_FACE('',(#1690),#1312,.T.);
#12970=ADVANCED_FACE('',(#1691),#1313,.T.);
#12971=ADVANCED_FACE('',(#1692),#1314,.T.);
#12972=ADVANCED_FACE('',(#1693),#1315,.T.);
#12973=ADVANCED_FACE('',(#1694),#1316,.F.);
#12974=ADVANCED_FACE('',(#1695),#12554,.F.);
#12975=ADVANCED_FACE('',(#1696),#12555,.F.);
#12976=ADVANCED_FACE('',(#1697),#12556,.F.);
#12977=ADVANCED_FACE('',(#1698),#12557,.F.);
#12978=ADVANCED_FACE('',(#1699),#12558,.F.);
#12979=ADVANCED_FACE('',(#1700),#12559,.F.);
#12980=ADVANCED_FACE('',(#1701),#12560,.F.);
#12981=ADVANCED_FACE('',(#1702),#12561,.F.);
#12982=ADVANCED_FACE('',(#1703),#12562,.F.);
#12983=ADVANCED_FACE('',(#1704,#1032,#1033),#1317,.T.);
#12984=ADVANCED_FACE('',(#1705,#1034,#1035),#1318,.T.);
#12985=ADVANCED_FACE('',(#1706),#1319,.T.);
#12986=ADVANCED_FACE('',(#1707),#1320,.T.);
#12987=ADVANCED_FACE('',(#1708,#1036,#1037,#1038,#1039,#1040),#1321,.T.);
#12988=ADVANCED_FACE('',(#1709),#1322,.T.);
#12989=ADVANCED_FACE('',(#1710,#1041,#1042,#1043,#1044,#1045),#1323,.T.);
#12990=ADVANCED_FACE('',(#1711),#1324,.T.);
#12991=ADVANCED_FACE('',(#1712),#1325,.T.);
#12992=ADVANCED_FACE('',(#1713,#1046,#1047,#1048,#1049),#1326,.F.);
#12993=ADVANCED_FACE('',(#1714),#12563,.F.);
#12994=ADVANCED_FACE('',(#1715),#12564,.T.);
#12995=ADVANCED_FACE('',(#1716,#1050),#1327,.T.);
#12996=ADVANCED_FACE('',(#1717,#1051),#1328,.F.);
#12997=ADVANCED_FACE('',(#1718),#12565,.F.);
#12998=ADVANCED_FACE('',(#1719),#12566,.F.);
#12999=ADVANCED_FACE('',(#1720),#12567,.F.);
#13000=ADVANCED_FACE('',(#1721),#12568,.F.);
#13001=ADVANCED_FACE('',(#1722,#1052),#1329,.F.);
#13002=ADVANCED_FACE('',(#1723),#12569,.T.);
#13003=ADVANCED_FACE('',(#1724),#12570,.T.);
#13004=ADVANCED_FACE('',(#1725),#12571,.T.);
#13005=ADVANCED_FACE('',(#1726),#12572,.T.);
#13006=ADVANCED_FACE('',(#1727),#12573,.T.);
#13007=ADVANCED_FACE('',(#1728,#1053),#1330,.T.);
#13008=ADVANCED_FACE('',(#1729),#12574,.F.);
#13009=ADVANCED_FACE('',(#1730,#1054),#1331,.T.);
#13010=ADVANCED_FACE('',(#1731),#12575,.F.);
#13011=ADVANCED_FACE('',(#1732),#12576,.F.);
#13012=ADVANCED_FACE('',(#1733),#12577,.F.);
#13013=ADVANCED_FACE('',(#1734),#12578,.F.);
#13014=ADVANCED_FACE('',(#1735,#1055),#1332,.F.);
#13015=ADVANCED_FACE('',(#1736),#12579,.T.);
#13016=ADVANCED_FACE('',(#1737),#12580,.T.);
#13017=ADVANCED_FACE('',(#1738),#12581,.T.);
#13018=ADVANCED_FACE('',(#1739),#12582,.T.);
#13019=ADVANCED_FACE('',(#1740),#12583,.T.);
#13020=ADVANCED_FACE('',(#1741,#1056),#1333,.F.);
#13021=ADVANCED_FACE('',(#1742),#12584,.F.);
#13022=ADVANCED_FACE('',(#1743,#1057),#1334,.T.);
#13023=ADVANCED_FACE('',(#1744),#12585,.F.);
#13024=ADVANCED_FACE('',(#1745),#12586,.F.);
#13025=ADVANCED_FACE('',(#1746,#1058,#1059,#1060,#1061,#1062),#1335,.T.);
#13026=ADVANCED_FACE('',(#1747),#12587,.F.);
#13027=ADVANCED_FACE('',(#1748),#1336,.T.);
#13028=ADVANCED_FACE('',(#1749),#1337,.T.);
#13029=ADVANCED_FACE('',(#1750),#1338,.T.);
#13030=ADVANCED_FACE('',(#1751),#1339,.T.);
#13031=ADVANCED_FACE('',(#1752),#12588,.F.);
#13032=ADVANCED_FACE('',(#1753),#12589,.F.);
#13033=ADVANCED_FACE('',(#1754),#12590,.F.);
#13034=ADVANCED_FACE('',(#1755),#12591,.F.);
#13035=ADVANCED_FACE('',(#1756),#12592,.F.);
#13036=ADVANCED_FACE('',(#1757),#12593,.F.);
#13037=ADVANCED_FACE('',(#1758),#12594,.F.);
#13038=ADVANCED_FACE('',(#1759),#12595,.F.);
#13039=ADVANCED_FACE('',(#1760),#12596,.F.);
#13040=ADVANCED_FACE('',(#1761,#1063,#1064),#1340,.T.);
#13041=ADVANCED_FACE('',(#1762,#1065,#1066),#1341,.T.);
#13042=ADVANCED_FACE('',(#1763),#1342,.T.);
#13043=ADVANCED_FACE('',(#1764),#1343,.T.);
#13044=ADVANCED_FACE('',(#1765,#1067,#1068,#1069,#1070,#1071),#1344,.T.);
#13045=ADVANCED_FACE('',(#1766),#1345,.T.);
#13046=ADVANCED_FACE('',(#1767),#1346,.T.);
#13047=ADVANCED_FACE('',(#1768,#1072,#1073,#1074,#1075),#1347,.F.);
#13048=ADVANCED_FACE('',(#1769),#12597,.F.);
#13049=ADVANCED_FACE('',(#1770),#12598,.T.);
#13050=ADVANCED_FACE('',(#1771,#1076),#1348,.T.);
#13051=ADVANCED_FACE('',(#1772,#1077),#1349,.F.);
#13052=ADVANCED_FACE('',(#1773),#12599,.F.);
#13053=ADVANCED_FACE('',(#1774),#12600,.T.);
#13054=ADVANCED_FACE('',(#1775,#1078),#1350,.T.);
#13055=ADVANCED_FACE('',(#1776,#1079),#1351,.F.);
#13056=ADVANCED_FACE('',(#1777),#12601,.F.);
#13057=ADVANCED_FACE('',(#1778),#12602,.T.);
#13058=ADVANCED_FACE('',(#1779,#1080),#1352,.T.);
#13059=ADVANCED_FACE('',(#1780,#1081),#1353,.F.);
#13060=ADVANCED_FACE('',(#1781),#12603,.F.);
#13061=ADVANCED_FACE('',(#1782),#12604,.T.);
#13062=ADVANCED_FACE('',(#1783,#1082),#1354,.T.);
#13063=ADVANCED_FACE('',(#1784,#1083),#1355,.F.);
#13064=ADVANCED_FACE('',(#1785),#12605,.F.);
#13065=ADVANCED_FACE('',(#1786),#12606,.T.);
#13066=ADVANCED_FACE('',(#1787,#1084),#1356,.T.);
#13067=ADVANCED_FACE('',(#1788,#1085),#1357,.F.);
#13068=ADVANCED_FACE('',(#1789),#12607,.F.);
#13069=ADVANCED_FACE('',(#1790),#12608,.F.);
#13070=ADVANCED_FACE('',(#1791),#12609,.F.);
#13071=ADVANCED_FACE('',(#1792),#12610,.F.);
#13072=ADVANCED_FACE('',(#1793,#1086),#1358,.F.);
#13073=ADVANCED_FACE('',(#1794),#12611,.T.);
#13074=ADVANCED_FACE('',(#1795),#12612,.T.);
#13075=ADVANCED_FACE('',(#1796),#12613,.T.);
#13076=ADVANCED_FACE('',(#1797),#12614,.T.);
#13077=ADVANCED_FACE('',(#1798),#12615,.T.);
#13078=ADVANCED_FACE('',(#1799,#1087),#1359,.T.);
#13079=ADVANCED_FACE('',(#1800),#12616,.F.);
#13080=ADVANCED_FACE('',(#1801,#1088),#1360,.T.);
#13081=ADVANCED_FACE('',(#1802),#12617,.F.);
#13082=ADVANCED_FACE('',(#1803),#1361,.T.);
#13083=ADVANCED_FACE('',(#1804),#1362,.T.);
#13084=ADVANCED_FACE('',(#1805),#12618,.F.);
#13085=ADVANCED_FACE('',(#1806),#1363,.T.);
#13086=ADVANCED_FACE('',(#1807),#12619,.F.);
#13087=ADVANCED_FACE('',(#1808),#1364,.T.);
#13088=ADVANCED_FACE('',(#1809),#12620,.F.);
#13089=ADVANCED_FACE('',(#1810),#12621,.F.);
#13090=ADVANCED_FACE('',(#1811),#12622,.F.);
#13091=ADVANCED_FACE('',(#1812),#12623,.F.);
#13092=ADVANCED_FACE('',(#1813),#12624,.T.);
#13093=ADVANCED_FACE('',(#1814,#1089),#1365,.T.);
#13094=ADVANCED_FACE('',(#1815,#1090),#1366,.F.);
#13095=ADVANCED_FACE('',(#1816),#12625,.T.);
#13096=ADVANCED_FACE('',(#1817),#12626,.T.);
#13097=ADVANCED_FACE('',(#1818),#12627,.F.);
#13098=ADVANCED_FACE('',(#1819),#12628,.T.);
#13099=ADVANCED_FACE('',(#1820),#12629,.F.);
#13100=ADVANCED_FACE('',(#1821),#1367,.F.);
#13101=ADVANCED_FACE('',(#1822),#1368,.F.);
#13102=ADVANCED_FACE('',(#1823,#1091),#1369,.F.);
#13103=ADVANCED_FACE('',(#1824),#12630,.F.);
#13104=ADVANCED_FACE('',(#1825),#12631,.F.);
#13105=ADVANCED_FACE('',(#1826),#12632,.T.);
#13106=ADVANCED_FACE('',(#1827),#1370,.T.);
#13107=ADVANCED_FACE('',(#1828),#1371,.T.);
#13108=ADVANCED_FACE('',(#1829),#12633,.T.);
#13109=ADVANCED_FACE('',(#1830,#1092),#1372,.T.);
#13110=ADVANCED_FACE('',(#1831),#12634,.F.);
#13111=ADVANCED_FACE('',(#1832,#1093),#1373,.T.);
#13112=ADVANCED_FACE('',(#1833),#12635,.F.);
#13113=ADVANCED_FACE('',(#1834),#12636,.F.);
#13114=ADVANCED_FACE('',(#1835,#1094),#1374,.T.);
#13115=ADVANCED_FACE('',(#1836),#12637,.F.);
#13116=ADVANCED_FACE('',(#1837),#12638,.F.);
#13117=ADVANCED_FACE('',(#1838,#1095),#1375,.T.);
#13118=ADVANCED_FACE('',(#1839),#12639,.F.);
#13119=ADVANCED_FACE('',(#1840),#12640,.F.);
#13120=ADVANCED_FACE('',(#1841,#1096),#1376,.T.);
#13121=ADVANCED_FACE('',(#1842),#12641,.F.);
#13122=ADVANCED_FACE('',(#1843),#12642,.F.);
#13123=ADVANCED_FACE('',(#1844),#1377,.T.);
#13124=ADVANCED_FACE('',(#1845),#12643,.F.);
#13125=ADVANCED_FACE('',(#1846),#1378,.T.);
#13126=ADVANCED_FACE('',(#1847),#1379,.T.);
#13127=ADVANCED_FACE('',(#1848),#1380,.T.);
#13128=ADVANCED_FACE('',(#1849),#1381,.T.);
#13129=ADVANCED_FACE('',(#1850),#1382,.T.);
#13130=ADVANCED_FACE('',(#1851,#1097,#1098,#1099,#1100,#1101,#1102),#1383,
 .T.);
#13131=ADVANCED_FACE('',(#1852,#1103,#1104,#1105,#1106),#1384,.F.);
#13132=ADVANCED_FACE('',(#1853),#12644,.F.);
#13133=ADVANCED_FACE('',(#1854),#12645,.T.);
#13134=ADVANCED_FACE('',(#1855,#1107),#1385,.T.);
#13135=ADVANCED_FACE('',(#1856,#1108),#1386,.F.);
#13136=ADVANCED_FACE('',(#1857),#12646,.F.);
#13137=ADVANCED_FACE('',(#1858),#12647,.T.);
#13138=ADVANCED_FACE('',(#1859,#1109),#1387,.T.);
#13139=ADVANCED_FACE('',(#1860,#1110),#1388,.F.);
#13140=ADVANCED_FACE('',(#1861),#12648,.F.);
#13141=ADVANCED_FACE('',(#1862,#1111),#1389,.T.);
#13142=ADVANCED_FACE('',(#1863),#12649,.F.);
#13143=ADVANCED_FACE('',(#1864),#12650,.F.);
#13144=ADVANCED_FACE('',(#1865,#1112),#1390,.T.);
#13145=ADVANCED_FACE('',(#1866),#12651,.F.);
#13146=ADVANCED_FACE('',(#1867),#12652,.F.);
#13147=ADVANCED_FACE('',(#1868,#1113),#1391,.T.);
#13148=ADVANCED_FACE('',(#1869),#12653,.F.);
#13149=ADVANCED_FACE('',(#1870),#12654,.F.);
#13150=ADVANCED_FACE('',(#1871,#1114),#1392,.T.);
#13151=ADVANCED_FACE('',(#1872),#12655,.F.);
#13152=ADVANCED_FACE('',(#1873),#12656,.F.);
#13153=ADVANCED_FACE('',(#1874),#1393,.T.);
#13154=ADVANCED_FACE('',(#1875),#12657,.F.);
#13155=ADVANCED_FACE('',(#1876),#1394,.T.);
#13156=ADVANCED_FACE('',(#1877),#1395,.T.);
#13157=ADVANCED_FACE('',(#1878),#1396,.T.);
#13158=ADVANCED_FACE('',(#1879),#1397,.T.);
#13159=ADVANCED_FACE('',(#1880),#1398,.T.);
#13160=ADVANCED_FACE('',(#1881,#1115,#1116,#1117,#1118,#1119,#1120),#1399,
 .T.);
#13161=ADVANCED_FACE('',(#1882,#1121,#1122,#1123,#1124),#1400,.F.);
#13162=ADVANCED_FACE('',(#1883),#12658,.F.);
#13163=ADVANCED_FACE('',(#1884),#12659,.T.);
#13164=ADVANCED_FACE('',(#1885,#1125),#1401,.T.);
#13165=ADVANCED_FACE('',(#1886,#1126),#1402,.F.);
#13166=ADVANCED_FACE('',(#1887),#12660,.F.);
#13167=ADVANCED_FACE('',(#1888),#12661,.T.);
#13168=ADVANCED_FACE('',(#1889,#1127),#1403,.T.);
#13169=ADVANCED_FACE('',(#1890,#1128),#1404,.F.);
#13170=ADVANCED_FACE('',(#1891),#12662,.F.);
#13171=ADVANCED_FACE('',(#1892,#1129),#1405,.T.);
#13172=ADVANCED_FACE('',(#1893),#12663,.F.);
#13173=ADVANCED_FACE('',(#1894),#12664,.F.);
#13174=ADVANCED_FACE('',(#1895,#1130),#1406,.T.);
#13175=ADVANCED_FACE('',(#1896),#12665,.F.);
#13176=ADVANCED_FACE('',(#1897),#1407,.T.);
#13177=ADVANCED_FACE('',(#1898),#1408,.T.);
#13178=ADVANCED_FACE('',(#1899),#1409,.T.);
#13179=ADVANCED_FACE('',(#1900),#1410,.T.);
#13180=ADVANCED_FACE('',(#1901,#1131,#1132),#1411,.T.);
#13181=ADVANCED_FACE('',(#1902,#1133,#1134),#1412,.F.);
#13182=ADVANCED_FACE('',(#1903),#1413,.T.);
#13183=ADVANCED_FACE('',(#1904),#1414,.T.);
#13184=ADVANCED_FACE('',(#1905),#1415,.T.);
#13185=ADVANCED_FACE('',(#1906),#1416,.T.);
#13186=ADVANCED_FACE('',(#1907),#1417,.T.);
#13187=ADVANCED_FACE('',(#1908),#1418,.F.);
#13188=ADVANCED_FACE('',(#1909),#12666,.F.);
#13189=ADVANCED_FACE('',(#1910),#12667,.F.);
#13190=ADVANCED_FACE('',(#1911,#1135,#1136),#1419,.T.);
#13191=ADVANCED_FACE('',(#1912),#1420,.T.);
#13192=ADVANCED_FACE('',(#1913,#1137,#1138),#1421,.T.);
#13193=ADVANCED_FACE('',(#1914),#1422,.T.);
#13194=ADVANCED_FACE('',(#1915),#1423,.T.);
#13195=ADVANCED_FACE('',(#1916),#1424,.F.);
#13196=ADVANCED_FACE('',(#1917),#12668,.F.);
#13197=ADVANCED_FACE('',(#1918),#12669,.F.);
#13198=ADVANCED_FACE('',(#1919,#1139,#1140),#1425,.T.);
#13199=ADVANCED_FACE('',(#1920),#1426,.T.);
#13200=ADVANCED_FACE('',(#1921,#1141,#1142),#1427,.T.);
#13201=ADVANCED_FACE('',(#1922),#1428,.T.);
#13202=ADVANCED_FACE('',(#1923),#1429,.T.);
#13203=ADVANCED_FACE('',(#1924),#1430,.F.);
#13204=ADVANCED_FACE('',(#1925),#12670,.F.);
#13205=ADVANCED_FACE('',(#1926),#12671,.F.);
#13206=ADVANCED_FACE('',(#1927),#12672,.F.);
#13207=ADVANCED_FACE('',(#1928),#12673,.F.);
#13208=ADVANCED_FACE('',(#1929),#1431,.T.);
#13209=ADVANCED_FACE('',(#1930),#1432,.T.);
#13210=ADVANCED_FACE('',(#1931),#1433,.T.);
#13211=ADVANCED_FACE('',(#1932),#1434,.T.);
#13212=ADVANCED_FACE('',(#1933,#1143,#1144,#1145,#1146),#1435,.T.);
#13213=ADVANCED_FACE('',(#1934,#1147,#1148,#1149,#1150),#1436,.F.);
#13214=ADVANCED_FACE('',(#1935),#705,.F.);
#13215=ADVANCED_FACE('',(#1936),#12674,.T.);
#13216=ADVANCED_FACE('',(#1937),#12675,.F.);
#13217=ADVANCED_FACE('',(#1938),#677,.F.);
#13218=ADVANCED_FACE('',(#1939,#1151),#1437,.T.);
#13219=ADVANCED_FACE('',(#1940),#12676,.T.);
#13220=ADVANCED_FACE('',(#1941,#1152),#1438,.T.);
#13221=ADVANCED_FACE('',(#1942),#678,.F.);
#13222=ADVANCED_FACE('',(#1943),#706,.F.);
#13223=ADVANCED_FACE('',(#1944),#12677,.F.);
#13224=ADVANCED_FACE('',(#1945,#1153),#1439,.T.);
#13225=ADVANCED_FACE('',(#1946),#679,.T.);
#13226=ADVANCED_FACE('',(#1947),#12678,.T.);
#13227=ADVANCED_FACE('',(#1948),#680,.T.);
#13228=ADVANCED_FACE('',(#1949,#1154),#1440,.T.);
#13229=ADVANCED_FACE('',(#1950),#12679,.F.);
#13230=ADVANCED_FACE('',(#1951),#645,.T.);
#13231=ADVANCED_FACE('',(#1952),#646,.T.);
#13232=ADVANCED_FACE('',(#1953),#647,.T.);
#13233=ADVANCED_FACE('',(#1954),#648,.T.);
#13234=ADVANCED_FACE('',(#1955),#649,.T.);
#13235=ADVANCED_FACE('',(#1956),#650,.T.);
#13236=ADVANCED_FACE('',(#1957),#651,.T.);
#13237=ADVANCED_FACE('',(#1958),#652,.T.);
#13238=ADVANCED_FACE('',(#1959),#653,.F.);
#13239=ADVANCED_FACE('',(#1960),#12680,.T.);
#13240=ADVANCED_FACE('',(#1961),#1441,.T.);
#13241=ADVANCED_FACE('',(#1962),#654,.F.);
#13242=ADVANCED_FACE('',(#1963),#1442,.T.);
#13243=ADVANCED_FACE('',(#1964),#655,.F.);
#13244=ADVANCED_FACE('',(#1965),#1443,.T.);
#13245=ADVANCED_FACE('',(#1966),#656,.F.);
#13246=ADVANCED_FACE('',(#1967),#1444,.T.);
#13247=ADVANCED_FACE('',(#1968),#657,.F.);
#13248=ADVANCED_FACE('',(#1969),#1445,.T.);
#13249=ADVANCED_FACE('',(#1970),#658,.F.);
#13250=ADVANCED_FACE('',(#1971),#1446,.T.);
#13251=ADVANCED_FACE('',(#1972),#659,.F.);
#13252=ADVANCED_FACE('',(#1973),#12681,.F.);
#13253=ADVANCED_FACE('',(#1974),#1447,.T.);
#13254=ADVANCED_FACE('',(#1975),#660,.F.);
#13255=ADVANCED_FACE('',(#1976,#1155),#1448,.T.);
#13256=ADVANCED_FACE('',(#1977),#1449,.T.);
#13257=ADVANCED_FACE('',(#1978,#1156),#1450,.T.);
#13258=ADVANCED_FACE('',(#1979),#12682,.T.);
#13259=ADVANCED_FACE('',(#1980,#1157),#1451,.T.);
#13260=ADVANCED_FACE('',(#1981),#12683,.F.);
#13261=ADVANCED_FACE('',(#1982,#1158),#1452,.T.);
#13262=ADVANCED_FACE('',(#1983),#12684,.T.);
#13263=ADVANCED_FACE('',(#1984,#1159),#1453,.T.);
#13264=ADVANCED_FACE('',(#1985),#12685,.F.);
#13265=ADVANCED_FACE('',(#1986),#1454,.F.);
#13266=ADVANCED_FACE('',(#1987),#1455,.F.);
#13267=ADVANCED_FACE('',(#1988),#1456,.F.);
#13268=ADVANCED_FACE('',(#1989),#1457,.F.);
#13269=ADVANCED_FACE('',(#1990),#1458,.F.);
#13270=ADVANCED_FACE('',(#1991),#1459,.F.);
#13271=ADVANCED_FACE('',(#1992),#1460,.F.);
#13272=ADVANCED_FACE('',(#1993),#1461,.F.);
#13273=ADVANCED_FACE('',(#1994,#1160),#1462,.T.);
#13274=ADVANCED_FACE('',(#1995),#12686,.T.);
#13275=ADVANCED_FACE('',(#1996),#1463,.F.);
#13276=ADVANCED_FACE('',(#1997),#1464,.T.);
#13277=ADVANCED_FACE('',(#1998),#681,.T.);
#13278=ADVANCED_FACE('',(#1999),#12687,.T.);
#13279=ADVANCED_FACE('',(#2000),#682,.T.);
#13280=ADVANCED_FACE('',(#2001,#1161),#1465,.T.);
#13281=ADVANCED_FACE('',(#2002),#683,.T.);
#13282=ADVANCED_FACE('',(#2003),#12688,.T.);
#13283=ADVANCED_FACE('',(#2004),#684,.T.);
#13284=ADVANCED_FACE('',(#2005),#707,.F.);
#13285=ADVANCED_FACE('',(#2006),#12689,.T.);
#13286=ADVANCED_FACE('',(#2007),#12690,.F.);
#13287=ADVANCED_FACE('',(#2008),#685,.F.);
#13288=ADVANCED_FACE('',(#2009,#1162),#1466,.T.);
#13289=ADVANCED_FACE('',(#2010),#12691,.T.);
#13290=ADVANCED_FACE('',(#2011,#1163),#1467,.T.);
#13291=ADVANCED_FACE('',(#2012),#686,.F.);
#13292=ADVANCED_FACE('',(#2013),#708,.F.);
#13293=ADVANCED_FACE('',(#2014),#12692,.F.);
#13294=ADVANCED_FACE('',(#2015,#1164),#1468,.T.);
#13295=ADVANCED_FACE('',(#2016),#687,.T.);
#13296=ADVANCED_FACE('',(#2017),#12693,.T.);
#13297=ADVANCED_FACE('',(#2018),#688,.T.);
#13298=ADVANCED_FACE('',(#2019,#1165),#1469,.T.);
#13299=ADVANCED_FACE('',(#2020),#12694,.F.);
#13300=ADVANCED_FACE('',(#2021),#661,.T.);
#13301=ADVANCED_FACE('',(#2022),#662,.T.);
#13302=ADVANCED_FACE('',(#2023),#663,.T.);
#13303=ADVANCED_FACE('',(#2024),#664,.T.);
#13304=ADVANCED_FACE('',(#2025),#665,.T.);
#13305=ADVANCED_FACE('',(#2026),#666,.T.);
#13306=ADVANCED_FACE('',(#2027),#667,.T.);
#13307=ADVANCED_FACE('',(#2028),#668,.F.);
#13308=ADVANCED_FACE('',(#2029),#12695,.T.);
#13309=ADVANCED_FACE('',(#2030),#1470,.T.);
#13310=ADVANCED_FACE('',(#2031),#669,.F.);
#13311=ADVANCED_FACE('',(#2032),#1471,.T.);
#13312=ADVANCED_FACE('',(#2033),#670,.F.);
#13313=ADVANCED_FACE('',(#2034),#1472,.T.);
#13314=ADVANCED_FACE('',(#2035),#671,.F.);
#13315=ADVANCED_FACE('',(#2036),#1473,.T.);
#13316=ADVANCED_FACE('',(#2037),#672,.F.);
#13317=ADVANCED_FACE('',(#2038),#1474,.T.);
#13318=ADVANCED_FACE('',(#2039),#673,.F.);
#13319=ADVANCED_FACE('',(#2040),#12696,.F.);
#13320=ADVANCED_FACE('',(#2041),#1475,.T.);
#13321=ADVANCED_FACE('',(#2042),#674,.F.);
#13322=ADVANCED_FACE('',(#2043,#1166),#1476,.T.);
#13323=ADVANCED_FACE('',(#2044),#1477,.T.);
#13324=ADVANCED_FACE('',(#2045,#1167),#1478,.T.);
#13325=ADVANCED_FACE('',(#2046),#12697,.T.);
#13326=ADVANCED_FACE('',(#2047,#1168),#1479,.T.);
#13327=ADVANCED_FACE('',(#2048),#12698,.F.);
#13328=ADVANCED_FACE('',(#2049,#1169),#1480,.T.);
#13329=ADVANCED_FACE('',(#2050),#12699,.T.);
#13330=ADVANCED_FACE('',(#2051,#1170),#1481,.T.);
#13331=ADVANCED_FACE('',(#2052),#12700,.F.);
#13332=ADVANCED_FACE('',(#2053),#1482,.T.);
#13333=ADVANCED_FACE('',(#2054),#689,.T.);
#13334=ADVANCED_FACE('',(#2055),#12701,.T.);
#13335=ADVANCED_FACE('',(#2056),#690,.T.);
#13336=ADVANCED_FACE('',(#2057,#1171),#1483,.T.);
#13337=ADVANCED_FACE('',(#2058),#691,.T.);
#13338=ADVANCED_FACE('',(#2059),#12702,.T.);
#13339=ADVANCED_FACE('',(#2060),#692,.T.);
#13340=ADVANCED_FACE('',(#2061),#1484,.T.);
#13341=ADVANCED_FACE('',(#2062),#1485,.F.);
#13342=ADVANCED_FACE('',(#2063),#1486,.F.);
#13343=ADVANCED_FACE('',(#2064),#1487,.F.);
#13344=ADVANCED_FACE('',(#2065),#1488,.F.);
#13345=ADVANCED_FACE('',(#2066),#1489,.F.);
#13346=ADVANCED_FACE('',(#2067),#1490,.F.);
#13347=ADVANCED_FACE('',(#2068),#1491,.F.);
#13348=ADVANCED_FACE('',(#2069),#1492,.F.);
#13349=ADVANCED_FACE('',(#2070),#12703,.F.);
#13350=ADVANCED_FACE('',(#2071),#12704,.F.);
#13351=ADVANCED_FACE('',(#2072,#1172,#1173),#675,.F.);
#13352=ADVANCED_FACE('',(#2073),#1493,.T.);
#13353=ADVANCED_FACE('',(#2074),#1494,.T.);
#13354=ADVANCED_FACE('',(#2075),#1495,.T.);
#13355=ADVANCED_FACE('',(#2076),#1496,.T.);
#13356=ADVANCED_FACE('',(#2077),#1497,.T.);
#13357=ADVANCED_FACE('',(#2078),#1498,.T.);
#13358=ADVANCED_FACE('',(#2079,#1174,#1175,#1176),#1499,.T.);
#13359=ADVANCED_FACE('',(#2080),#12705,.T.);
#13360=ADVANCED_FACE('',(#2081,#1177),#1500,.F.);
#13361=ADVANCED_FACE('',(#2082,#1178),#1501,.T.);
#13362=ADVANCED_FACE('',(#2083),#1502,.F.);
#13363=ADVANCED_FACE('',(#2084),#1503,.F.);
#13364=ADVANCED_FACE('',(#2085),#1504,.F.);
#13365=ADVANCED_FACE('',(#2086),#1505,.F.);
#13366=ADVANCED_FACE('',(#2087),#1506,.F.);
#13367=ADVANCED_FACE('',(#2088),#12706,.F.);
#13368=ADVANCED_FACE('',(#2089),#12707,.F.);
#13369=ADVANCED_FACE('',(#2090),#1507,.T.);
#13370=ADVANCED_FACE('',(#2091),#1508,.T.);
#13371=ADVANCED_FACE('',(#2092),#1509,.T.);
#13372=ADVANCED_FACE('',(#2093),#1510,.T.);
#13373=ADVANCED_FACE('',(#2094,#1179,#1180,#1181),#1511,.F.);
#13374=ADVANCED_FACE('',(#2095),#12708,.F.);
#13375=ADVANCED_FACE('',(#2096,#1182),#1512,.T.);
#13376=ADVANCED_FACE('',(#2097,#1183,#1184),#676,.T.);
#13377=ADVANCED_FACE('',(#2098,#1185),#1513,.T.);
#13378=ADVANCED_FACE('',(#2099),#12709,.F.);
#13379=ADVANCED_FACE('',(#2100),#12710,.F.);
#13380=ADVANCED_FACE('',(#2101,#1186,#1187,#1188,#1189,#1190,#1191),#12711,
 .T.);
#13381=ADVANCED_FACE('',(#2102),#12712,.F.);
#13382=ADVANCED_FACE('',(#2103),#12713,.F.);
#13383=ADVANCED_FACE('',(#2104),#12714,.F.);
#13384=ADVANCED_FACE('',(#2105),#12715,.F.);
#13385=ADVANCED_FACE('',(#2106,#1192),#1514,.T.);
#13386=ADVANCED_FACE('',(#2107,#1193),#1515,.T.);
#13387=ADVANCED_FACE('',(#2108),#12716,.T.);
#13388=ADVANCED_FACE('',(#2109,#1194),#1516,.T.);
#13389=ADVANCED_FACE('',(#2110,#1195,#1196,#1197,#1198,#1199,#1200),#12717,
 .F.);
#13390=ADVANCED_FACE('',(#2111),#12718,.F.);
#13391=ADVANCED_FACE('',(#2112),#12719,.T.);
#13392=ADVANCED_FACE('',(#2113,#1201),#1517,.T.);
#13393=ADVANCED_FACE('',(#2114,#1202),#1518,.F.);
#13394=ADVANCED_FACE('',(#2115),#1519,.F.);
#13395=ADVANCED_FACE('',(#2116),#1520,.F.);
#13396=ADVANCED_FACE('',(#2117),#1521,.F.);
#13397=ADVANCED_FACE('',(#2118),#1522,.F.);
#13398=ADVANCED_FACE('',(#2119),#1523,.F.);
#13399=ADVANCED_FACE('',(#2120),#1524,.F.);
#13400=ADVANCED_FACE('',(#2121),#1525,.F.);
#13401=ADVANCED_FACE('',(#2122),#1526,.F.);
#13402=ADVANCED_FACE('',(#2123),#1527,.F.);
#13403=ADVANCED_FACE('',(#2124),#1528,.T.);
#13404=ADVANCED_FACE('',(#2125),#693,.T.);
#13405=ADVANCED_FACE('',(#2126),#12720,.T.);
#13406=ADVANCED_FACE('',(#2127),#694,.T.);
#13407=ADVANCED_FACE('',(#2128,#1203),#1529,.T.);
#13408=ADVANCED_FACE('',(#2129),#695,.T.);
#13409=ADVANCED_FACE('',(#2130),#12721,.T.);
#13410=ADVANCED_FACE('',(#2131),#1530,.F.);
#13411=ADVANCED_FACE('',(#2132),#1531,.F.);
#13412=ADVANCED_FACE('',(#2133),#1532,.F.);
#13413=ADVANCED_FACE('',(#2134),#1533,.F.);
#13414=ADVANCED_FACE('',(#2135),#1534,.F.);
#13415=ADVANCED_FACE('',(#2136),#1535,.F.);
#13416=ADVANCED_FACE('',(#2137),#1536,.F.);
#13417=ADVANCED_FACE('',(#2138),#1537,.F.);
#13418=ADVANCED_FACE('',(#2139),#1538,.F.);
#13419=ADVANCED_FACE('',(#2140),#1539,.T.);
#13420=ADVANCED_FACE('',(#2141),#696,.T.);
#13421=ADVANCED_FACE('',(#2142),#12722,.T.);
#13422=ADVANCED_FACE('',(#2143),#697,.T.);
#13423=ADVANCED_FACE('',(#2144,#1204),#1540,.T.);
#13424=ADVANCED_FACE('',(#2145),#698,.T.);
#13425=ADVANCED_FACE('',(#2146),#12723,.T.);
#13426=ADVANCED_FACE('',(#2147),#12724,.F.);
#13427=ADVANCED_FACE('',(#2148),#1541,.F.);
#13428=ADVANCED_FACE('',(#2149,#1205),#1542,.T.);
#13429=ADVANCED_FACE('',(#2150,#1206),#1543,.F.);
#13430=ADVANCED_FACE('',(#2151),#12725,.T.);
#13431=ADVANCED_FACE('',(#2152),#12726,.T.);
#13432=ADVANCED_FACE('',(#2153),#12727,.T.);
#13433=ADVANCED_FACE('',(#2154,#1207),#1544,.F.);
#13434=ADVANCED_FACE('',(#2155),#12728,.T.);
#13435=ADVANCED_FACE('',(#2156),#1545,.T.);
#13436=ADVANCED_FACE('',(#2157,#1208),#1546,.F.);
#13437=ADVANCED_FACE('',(#2158),#12729,.F.);
#13438=ADVANCED_FACE('',(#2159,#1209),#1547,.T.);
#13439=ADVANCED_FACE('',(#2160),#12730,.F.);
#13440=ADVANCED_FACE('',(#2161),#12731,.T.);
#13441=ADVANCED_FACE('',(#2162,#1210),#1548,.T.);
#13442=ADVANCED_FACE('',(#2163,#1211),#1549,.F.);
#13443=ADVANCED_FACE('',(#2164),#12732,.F.);
#13444=ADVANCED_FACE('',(#2165),#12733,.T.);
#13445=ADVANCED_FACE('',(#2166,#1212),#1550,.T.);
#13446=ADVANCED_FACE('',(#2167,#1213),#1551,.F.);
#13447=ADVANCED_FACE('',(#2168),#12734,.T.);
#13448=ADVANCED_FACE('',(#2169),#1552,.T.);
#13449=ADVANCED_FACE('',(#2170),#1553,.F.);
#13450=ADVANCED_FACE('',(#2171),#12735,.T.);
#13451=ADVANCED_FACE('',(#2172),#1554,.T.);
#13452=ADVANCED_FACE('',(#2173),#1555,.F.);
#13453=ADVANCED_FACE('',(#2174),#12736,.F.);
#13454=ADVANCED_FACE('',(#2175),#12737,.T.);
#13455=ADVANCED_FACE('',(#2176,#1214),#1556,.T.);
#13456=ADVANCED_FACE('',(#2177,#1215),#1557,.F.);
#13457=ADVANCED_FACE('',(#2178),#12738,.T.);
#13458=ADVANCED_FACE('',(#2179),#1558,.T.);
#13459=ADVANCED_FACE('',(#2180),#1559,.F.);
#13460=ADVANCED_FACE('',(#2181),#1560,.T.);
#13461=ADVANCED_FACE('',(#2182),#12739,.F.);
#13462=ADVANCED_FACE('',(#2183),#1561,.T.);
#13463=ADVANCED_FACE('',(#2184),#1562,.T.);
#13464=ADVANCED_FACE('',(#2185),#12740,.F.);
#13465=ADVANCED_FACE('',(#2186),#1563,.T.);
#13466=ADVANCED_FACE('',(#2187,#1216,#1217),#12741,.F.);
#13467=ADVANCED_FACE('',(#2188,#1218,#1219),#12742,.T.);
#13468=ADVANCED_FACE('',(#2189,#1220),#1564,.T.);
#13469=ADVANCED_FACE('',(#2190,#1221),#1565,.F.);
#13470=ADVANCED_FACE('',(#2191),#12743,.F.);
#13471=ADVANCED_FACE('',(#2192),#12744,.F.);
#13472=ADVANCED_FACE('',(#2193,#1222,#1223,#1224),#12745,.T.);
#13473=ADVANCED_FACE('',(#2194),#12746,.F.);
#13474=ADVANCED_FACE('',(#2195),#12747,.F.);
#13475=ADVANCED_FACE('',(#2196,#1225,#1226,#1227),#12748,.F.);
#13476=ADVANCED_FACE('',(#2197,#1228),#1566,.F.);
#13477=ADVANCED_FACE('',(#2198,#1229),#1567,.T.);
#13478=ADVANCED_FACE('',(#2199),#12749,.T.);
#13479=ADVANCED_FACE('',(#2200,#1230),#1568,.F.);
#13480=ADVANCED_FACE('',(#2201,#1231),#1569,.F.);
#13481=ADVANCED_FACE('',(#2202),#12750,.T.);
#13482=ADVANCED_FACE('',(#2203,#1232),#1570,.T.);
#13483=ADVANCED_FACE('',(#2204),#12751,.F.);
#13484=ADVANCED_FACE('',(#2205),#12752,.T.);
#13485=ADVANCED_FACE('',(#2206),#12753,.F.);
#13486=ADVANCED_FACE('',(#2207),#12754,.T.);
#13487=ADVANCED_FACE('',(#2208),#12755,.F.);
#13488=ADVANCED_FACE('',(#2209),#12756,.T.);
#13489=ADVANCED_FACE('',(#2210),#12757,.F.);
#13490=ADVANCED_FACE('',(#2211),#12758,.T.);
#13491=ADVANCED_FACE('',(#2212),#12759,.F.);
#13492=ADVANCED_FACE('',(#2213),#12760,.T.);
#13493=ADVANCED_FACE('',(#2214),#12761,.F.);
#13494=ADVANCED_FACE('',(#2215),#12762,.T.);
#13495=ADVANCED_FACE('',(#2216),#12763,.F.);
#13496=ADVANCED_FACE('',(#2217),#12764,.T.);
#13497=ADVANCED_FACE('',(#2218),#12765,.F.);
#13498=ADVANCED_FACE('',(#2219),#12766,.T.);
#13499=ADVANCED_FACE('',(#2220),#12767,.F.);
#13500=ADVANCED_FACE('',(#2221),#12768,.T.);
#13501=ADVANCED_FACE('',(#2222),#12769,.F.);
#13502=ADVANCED_FACE('',(#2223),#12770,.T.);
#13503=ADVANCED_FACE('',(#2224),#12771,.F.);
#13504=ADVANCED_FACE('',(#2225),#12772,.T.);
#13505=ADVANCED_FACE('',(#2226),#12773,.F.);
#13506=ADVANCED_FACE('',(#2227),#12774,.T.);
#13507=ADVANCED_FACE('',(#2228),#12775,.F.);
#13508=ADVANCED_FACE('',(#2229),#12776,.T.);
#13509=ADVANCED_FACE('',(#2230),#12777,.F.);
#13510=ADVANCED_FACE('',(#2231),#12778,.T.);
#13511=ADVANCED_FACE('',(#2232),#12779,.F.);
#13512=ADVANCED_FACE('',(#2233),#12780,.T.);
#13513=ADVANCED_FACE('',(#2234),#12781,.F.);
#13514=ADVANCED_FACE('',(#2235),#12782,.T.);
#13515=ADVANCED_FACE('',(#2236),#12783,.F.);
#13516=ADVANCED_FACE('',(#2237),#12784,.T.);
#13517=ADVANCED_FACE('',(#2238),#12785,.F.);
#13518=ADVANCED_FACE('',(#2239),#12786,.T.);
#13519=ADVANCED_FACE('',(#2240),#12787,.F.);
#13520=ADVANCED_FACE('',(#2241),#12788,.T.);
#13521=ADVANCED_FACE('',(#2242),#12789,.F.);
#13522=ADVANCED_FACE('',(#2243),#12790,.T.);
#13523=ADVANCED_FACE('',(#2244,#1233),#1571,.F.);
#13524=ADVANCED_FACE('',(#2245),#12791,.T.);
#13525=ADVANCED_FACE('',(#2246),#1572,.T.);
#13526=ADVANCED_FACE('',(#2247),#12792,.F.);
#13527=ADVANCED_FACE('',(#2248),#1573,.F.);
#13528=ADVANCED_FACE('',(#2249,#1234),#1574,.F.);
#13529=ADVANCED_FACE('',(#2250),#12793,.T.);
#13530=ADVANCED_FACE('',(#2251),#12794,.T.);
#13531=ADVANCED_FACE('',(#2252,#1235),#1575,.F.);
#13532=ADVANCED_FACE('',(#2253),#12795,.F.);
#13533=ADVANCED_FACE('',(#2254),#12796,.T.);
#13534=ADVANCED_FACE('',(#2255,#1236),#1576,.T.);
#13535=ADVANCED_FACE('',(#2256,#1237),#1577,.F.);
#13536=ADVANCED_FACE('',(#2257),#12797,.F.);
#13537=ADVANCED_FACE('',(#2258),#12798,.T.);
#13538=ADVANCED_FACE('',(#2259,#1238),#1578,.T.);
#13539=ADVANCED_FACE('',(#2260,#1239),#1579,.F.);
#13540=ADVANCED_FACE('',(#2261),#12799,.T.);
#13541=ADVANCED_FACE('',(#2262),#1580,.T.);
#13542=ADVANCED_FACE('',(#2263),#1581,.F.);
#13543=ADVANCED_FACE('',(#2264),#12800,.T.);
#13544=ADVANCED_FACE('',(#2265),#1582,.T.);
#13545=ADVANCED_FACE('',(#2266),#1583,.F.);
#13546=ADVANCED_FACE('',(#2267),#12801,.F.);
#13547=ADVANCED_FACE('',(#2268),#12802,.T.);
#13548=ADVANCED_FACE('',(#2269,#1240),#1584,.T.);
#13549=ADVANCED_FACE('',(#2270,#1241),#1585,.F.);
#13550=ADVANCED_FACE('',(#2271),#1586,.T.);
#13551=ADVANCED_FACE('',(#2272),#12803,.F.);
#13552=ADVANCED_FACE('',(#2273),#1587,.T.);
#13553=ADVANCED_FACE('',(#2274,#1242),#12804,.F.);
#13554=ADVANCED_FACE('',(#2275,#1243),#12805,.T.);
#13555=ADVANCED_FACE('',(#2276,#1244),#1588,.T.);
#13556=ADVANCED_FACE('',(#2277,#1245),#1589,.F.);
#13557=ADVANCED_FACE('',(#2278),#1590,.T.);
#13558=ADVANCED_FACE('',(#2279),#12806,.F.);
#13559=ADVANCED_FACE('',(#2280),#1591,.T.);
#13560=ADVANCED_FACE('',(#2281,#1246),#12807,.F.);
#13561=ADVANCED_FACE('',(#2282,#1247),#12808,.T.);
#13562=ADVANCED_FACE('',(#2283,#1248),#1592,.T.);
#13563=ADVANCED_FACE('',(#2284,#1249),#1593,.F.);
#13564=ADVANCED_FACE('',(#2285),#12809,.F.);
#13565=ADVANCED_FACE('',(#2286),#12810,.T.);
#13566=ADVANCED_FACE('',(#2287,#1250),#1594,.T.);
#13567=ADVANCED_FACE('',(#2288,#1251),#1595,.F.);
#13568=ADVANCED_FACE('',(#2289),#12811,.F.);
#13569=ADVANCED_FACE('',(#2290),#12812,.T.);
#13570=ADVANCED_FACE('',(#2291,#1252),#1596,.T.);
#13571=ADVANCED_FACE('',(#2292,#1253),#1597,.F.);
#13572=ADVANCED_FACE('',(#2293),#12813,.F.);
#13573=ADVANCED_FACE('',(#2294),#12814,.T.);
#13574=ADVANCED_FACE('',(#2295,#1254),#1598,.T.);
#13575=ADVANCED_FACE('',(#2296,#1255),#1599,.F.);
#13576=ADVANCED_FACE('',(#2297),#1600,.T.);
#13577=ADVANCED_FACE('',(#2298),#12815,.F.);
#13578=ADVANCED_FACE('',(#2299),#1601,.T.);
#13579=ADVANCED_FACE('',(#2300,#1256),#12816,.F.);
#13580=ADVANCED_FACE('',(#2301,#1257),#12817,.T.);
#13581=ADVANCED_FACE('',(#2302,#1258),#1602,.T.);
#13582=ADVANCED_FACE('',(#2303,#1259),#1603,.F.);
#13583=ADVANCED_FACE('',(#2304),#1604,.T.);
#13584=ADVANCED_FACE('',(#2305),#12818,.F.);
#13585=ADVANCED_FACE('',(#2306),#1605,.T.);
#13586=ADVANCED_FACE('',(#2307,#1260),#12819,.F.);
#13587=ADVANCED_FACE('',(#2308,#1261),#12820,.T.);
#13588=ADVANCED_FACE('',(#2309,#1262),#1606,.T.);
#13589=ADVANCED_FACE('',(#2310,#1263),#1607,.F.);
#13590=ADVANCED_FACE('',(#2311),#12821,.F.);
#13591=ADVANCED_FACE('',(#2312),#12822,.F.);
#13592=ADVANCED_FACE('',(#2313,#1264,#1265,#1266),#12823,.T.);
#13593=ADVANCED_FACE('',(#2314),#12824,.F.);
#13594=ADVANCED_FACE('',(#2315),#12825,.F.);
#13595=ADVANCED_FACE('',(#2316,#1267,#1268,#1269),#12826,.F.);
#13596=ADVANCED_FACE('',(#2317,#1270),#1608,.F.);
#13597=ADVANCED_FACE('',(#2318,#1271),#1609,.T.);
#13598=ADVANCED_FACE('',(#2319),#12827,.T.);
#13599=ADVANCED_FACE('',(#2320,#1272),#1610,.F.);
#13600=ADVANCED_FACE('',(#2321,#1273),#1611,.F.);
#13601=ADVANCED_FACE('',(#2322),#12828,.T.);
#13602=ADVANCED_FACE('',(#2323,#1274),#1612,.T.);
#13603=ADVANCED_FACE('',(#2324),#12829,.F.);
#13604=ADVANCED_FACE('',(#2325),#12830,.T.);
#13605=ADVANCED_FACE('',(#2326),#12831,.F.);
#13606=ADVANCED_FACE('',(#2327),#12832,.T.);
#13607=ADVANCED_FACE('',(#2328),#12833,.F.);
#13608=ADVANCED_FACE('',(#2329),#12834,.T.);
#13609=ADVANCED_FACE('',(#2330),#12835,.F.);
#13610=ADVANCED_FACE('',(#2331),#12836,.T.);
#13611=ADVANCED_FACE('',(#2332),#12837,.F.);
#13612=ADVANCED_FACE('',(#2333),#12838,.T.);
#13613=ADVANCED_FACE('',(#2334),#12839,.F.);
#13614=ADVANCED_FACE('',(#2335),#12840,.T.);
#13615=ADVANCED_FACE('',(#2336),#12841,.F.);
#13616=ADVANCED_FACE('',(#2337),#12842,.T.);
#13617=ADVANCED_FACE('',(#2338),#12843,.F.);
#13618=ADVANCED_FACE('',(#2339),#12844,.T.);
#13619=ADVANCED_FACE('',(#2340),#12845,.F.);
#13620=ADVANCED_FACE('',(#2341),#12846,.T.);
#13621=ADVANCED_FACE('',(#2342),#12847,.F.);
#13622=ADVANCED_FACE('',(#2343),#12848,.T.);
#13623=ADVANCED_FACE('',(#2344),#12849,.F.);
#13624=ADVANCED_FACE('',(#2345),#12850,.T.);
#13625=ADVANCED_FACE('',(#2346),#12851,.F.);
#13626=ADVANCED_FACE('',(#2347),#12852,.T.);
#13627=ADVANCED_FACE('',(#2348),#12853,.F.);
#13628=ADVANCED_FACE('',(#2349),#12854,.T.);
#13629=ADVANCED_FACE('',(#2350),#12855,.F.);
#13630=ADVANCED_FACE('',(#2351),#12856,.T.);
#13631=ADVANCED_FACE('',(#2352),#12857,.F.);
#13632=ADVANCED_FACE('',(#2353),#12858,.T.);
#13633=ADVANCED_FACE('',(#2354),#12859,.F.);
#13634=ADVANCED_FACE('',(#2355),#12860,.T.);
#13635=ADVANCED_FACE('',(#2356),#12861,.F.);
#13636=ADVANCED_FACE('',(#2357),#12862,.T.);
#13637=ADVANCED_FACE('',(#2358),#12863,.F.);
#13638=ADVANCED_FACE('',(#2359),#12864,.T.);
#13639=ADVANCED_FACE('',(#2360),#12865,.F.);
#13640=ADVANCED_FACE('',(#2361),#12866,.T.);
#13641=ADVANCED_FACE('',(#2362),#12867,.F.);
#13642=ADVANCED_FACE('',(#2363),#12868,.T.);
#13643=ADVANCED_FACE('',(#2364),#12869,.F.);
#13644=ADVANCED_FACE('',(#2365),#12870,.T.);
#13645=ADVANCED_FACE('',(#2366),#12871,.F.);
#13646=ADVANCED_FACE('',(#2367),#12872,.T.);
#13647=ADVANCED_FACE('',(#2368),#12873,.F.);
#13648=ADVANCED_FACE('',(#2369),#12874,.T.);
#13649=ADVANCED_FACE('',(#2370),#12875,.F.);
#13650=ADVANCED_FACE('',(#2371),#12876,.T.);
#13651=ADVANCED_FACE('',(#2372),#12877,.F.);
#13652=ADVANCED_FACE('',(#2373),#12878,.T.);
#13653=ADVANCED_FACE('',(#2374),#12879,.F.);
#13654=ADVANCED_FACE('',(#2375),#12880,.T.);
#13655=ADVANCED_FACE('',(#2376),#12881,.F.);
#13656=ADVANCED_FACE('',(#2377),#12882,.T.);
#13657=ADVANCED_FACE('',(#2378),#12883,.F.);
#13658=ADVANCED_FACE('',(#2379),#12884,.T.);
#13659=ADVANCED_FACE('',(#2380),#12885,.F.);
#13660=ADVANCED_FACE('',(#2381),#12886,.T.);
#13661=ADVANCED_FACE('',(#2382),#12887,.F.);
#13662=ADVANCED_FACE('',(#2383),#12888,.T.);
#13663=ADVANCED_FACE('',(#2384),#12889,.F.);
#13664=ADVANCED_FACE('',(#2385),#12890,.T.);
#13665=ADVANCED_FACE('',(#2386),#12891,.F.);
#13666=ADVANCED_FACE('',(#2387),#12892,.T.);
#13667=ADVANCED_FACE('',(#2388),#12893,.F.);
#13668=ADVANCED_FACE('',(#2389),#12894,.T.);
#13669=ADVANCED_FACE('',(#2390),#12895,.F.);
#13670=ADVANCED_FACE('',(#2391),#12896,.T.);
#13671=ADVANCED_FACE('',(#2392),#12897,.F.);
#13672=ADVANCED_FACE('',(#2393),#12898,.T.);
#13673=ADVANCED_FACE('',(#2394),#12899,.F.);
#13674=ADVANCED_FACE('',(#2395),#12900,.T.);
#13675=ADVANCED_FACE('',(#2396),#12901,.F.);
#13676=ADVANCED_FACE('',(#2397),#12902,.T.);
#13677=ADVANCED_FACE('',(#2398),#12903,.F.);
#13678=ADVANCED_FACE('',(#2399),#12904,.T.);
#13679=ADVANCED_FACE('',(#2400),#12905,.F.);
#13680=ADVANCED_FACE('',(#2401),#12906,.T.);
#13681=ADVANCED_FACE('',(#2402),#12907,.F.);
#13682=ADVANCED_FACE('',(#2403),#12908,.T.);
#13683=ADVANCED_FACE('',(#2404),#1613,.T.);
#13684=ADVANCED_FACE('',(#2405),#699,.T.);
#13685=ADVANCED_FACE('',(#2406),#12909,.T.);
#13686=ADVANCED_FACE('',(#2407),#700,.T.);
#13687=ADVANCED_FACE('',(#2408,#1275),#1614,.T.);
#13688=ADVANCED_FACE('',(#2409),#701,.T.);
#13689=ADVANCED_FACE('',(#2410),#12910,.T.);
#13690=ADVANCED_FACE('',(#2411),#702,.T.);
#13691=ADVANCED_FACE('',(#2412),#1615,.T.);
#13692=ADVANCED_FACE('',(#2413),#1616,.F.);
#13693=ADVANCED_FACE('',(#2414),#1617,.F.);
#13694=ADVANCED_FACE('',(#2415),#1618,.F.);
#13695=ADVANCED_FACE('',(#2416),#1619,.F.);
#13696=ADVANCED_FACE('',(#2417),#1620,.F.);
#13697=ADVANCED_FACE('',(#2418),#1621,.F.);
#13698=ADVANCED_FACE('',(#2419),#1622,.F.);
#13699=ADVANCED_FACE('',(#2420),#1623,.F.);
#13700=ADVANCED_FACE('',(#2421),#1624,.F.);
#13701=ADVANCED_FACE('',(#2422),#1625,.F.);
#13702=ADVANCED_FACE('',(#2423),#1626,.F.);
#13703=ADVANCED_FACE('',(#2424),#1627,.F.);
#13704=ADVANCED_FACE('',(#2425),#1628,.F.);
#13705=ADVANCED_FACE('',(#2426),#1629,.F.);
#13706=ADVANCED_FACE('',(#2427),#1630,.F.);
#13707=ADVANCED_FACE('',(#2428,#1276),#1631,.T.);
#13708=ADVANCED_FACE('',(#2429),#703,.T.);
#13709=ADVANCED_FACE('',(#2430),#12911,.T.);
#13710=ADVANCED_FACE('',(#2431),#704,.T.);
#13711=ADVANCED_FACE('',(#2432),#1632,.T.);
#13712=CLOSED_SHELL('',(#12912,#12913,#12914,#12915,#12916,#12917,#12918,
#12919,#12920,#12921,#12922,#12923,#12924,#12925,#12926,#12927,#12928,#12929,
#12930,#12931,#12932,#12933,#12934,#12935,#12936,#12937,#12938,#12939,#12940,
#12941,#12942,#12943,#12944,#12945,#12946,#12947,#12948,#12949,#12950,#12951,
#12952,#12953,#12954,#12955,#12956,#12957,#12958,#12959,#12960,#12961));
#13713=CLOSED_SHELL('',(#12962,#12963,#12964,#12965,#12966,#12967));
#13714=CLOSED_SHELL('',(#12968,#12969,#12970,#12971,#12972,#12973));
#13715=CLOSED_SHELL('',(#12974,#12975,#12976,#12977,#12978,#12979,#12980,
#12981,#12982,#12983,#12984,#12985,#12986,#12987,#12988,#12989,#12990,#12991,
#12992));
#13716=CLOSED_SHELL('',(#12993,#12994,#12995,#12996));
#13717=CLOSED_SHELL('',(#12997,#12998,#12999,#13000,#13001,#13002,#13003,
#13004,#13005,#13006,#13007,#13008,#13009));
#13718=CLOSED_SHELL('',(#13010,#13011,#13012,#13013,#13014,#13015,#13016,
#13017,#13018,#13019,#13020,#13021,#13022));
#13719=CLOSED_SHELL('',(#13023,#13024,#13025,#13026,#13027,#13028,#13029,
#13030,#13031,#13032,#13033,#13034,#13035,#13036,#13037,#13038,#13039,#13040,
#13041,#13042,#13043,#13044,#13045,#13046,#13047));
#13720=CLOSED_SHELL('',(#13048,#13049,#13050,#13051));
#13721=CLOSED_SHELL('',(#13052,#13053,#13054,#13055));
#13722=CLOSED_SHELL('',(#13056,#13057,#13058,#13059));
#13723=CLOSED_SHELL('',(#13060,#13061,#13062,#13063));
#13724=CLOSED_SHELL('',(#13064,#13065,#13066,#13067));
#13725=CLOSED_SHELL('',(#13068,#13069,#13070,#13071,#13072,#13073,#13074,
#13075,#13076,#13077,#13078,#13079,#13080));
#13726=CLOSED_SHELL('',(#13081,#13082,#13083,#13084,#13085,#13086,#13087,
#13088,#13089,#13090,#13091,#13092,#13093,#13094,#13095,#13096,#13097,#13098,
#13099));
#13727=CLOSED_SHELL('',(#13100,#13101,#13102,#13103,#13104,#13105,#13106,
#13107,#13108,#13109));
#13728=CLOSED_SHELL('',(#13110,#13111,#13112,#13113,#13114,#13115,#13116,
#13117,#13118,#13119,#13120,#13121,#13122,#13123,#13124,#13125,#13126,#13127,
#13128,#13129,#13130,#13131));
#13729=CLOSED_SHELL('',(#13132,#13133,#13134,#13135));
#13730=CLOSED_SHELL('',(#13136,#13137,#13138,#13139));
#13731=CLOSED_SHELL('',(#13140,#13141,#13142,#13143,#13144,#13145,#13146,
#13147,#13148,#13149,#13150,#13151,#13152,#13153,#13154,#13155,#13156,#13157,
#13158,#13159,#13160,#13161));
#13732=CLOSED_SHELL('',(#13162,#13163,#13164,#13165));
#13733=CLOSED_SHELL('',(#13166,#13167,#13168,#13169));
#13734=CLOSED_SHELL('',(#13170,#13171,#13172,#13173,#13174,#13175,#13176,
#13177,#13178,#13179,#13180,#13181));
#13735=CLOSED_SHELL('',(#13182,#13183,#13184,#13185,#13186,#13187));
#13736=CLOSED_SHELL('',(#13188,#13189,#13190,#13191,#13192,#13193,#13194,
#13195));
#13737=CLOSED_SHELL('',(#13196,#13197,#13198,#13199,#13200,#13201,#13202,
#13203));
#13738=CLOSED_SHELL('',(#13204,#13205,#13206,#13207,#13208,#13209,#13210,
#13211,#13212,#13213));
#13739=CLOSED_SHELL('',(#13214,#13215,#13216,#13217,#13218,#13219,#13220,
#13221));
#13740=CLOSED_SHELL('',(#13222,#13223,#13224,#13225,#13226,#13227,#13228,
#13229));
#13741=CLOSED_SHELL('',(#13230));
#13742=CLOSED_SHELL('',(#13231));
#13743=CLOSED_SHELL('',(#13232));
#13744=CLOSED_SHELL('',(#13233));
#13745=CLOSED_SHELL('',(#13234));
#13746=CLOSED_SHELL('',(#13235));
#13747=CLOSED_SHELL('',(#13236));
#13748=CLOSED_SHELL('',(#13237));
#13749=CLOSED_SHELL('',(#13238,#13239,#13240,#13241,#13242,#13243,#13244,
#13245,#13246,#13247,#13248,#13249,#13250,#13251,#13252,#13253,#13254,#13255,
#13256));
#13750=CLOSED_SHELL('',(#13257,#13258,#13259,#13260));
#13751=CLOSED_SHELL('',(#13261,#13262,#13263,#13264));
#13752=CLOSED_SHELL('',(#13265,#13266,#13267,#13268,#13269,#13270,#13271,
#13272));
#13753=CLOSED_SHELL('',(#13273,#13274,#13275,#13276,#13277,#13278,#13279,
#13280,#13281,#13282,#13283));
#13754=CLOSED_SHELL('',(#13284,#13285,#13286,#13287,#13288,#13289,#13290,
#13291));
#13755=CLOSED_SHELL('',(#13292,#13293,#13294,#13295,#13296,#13297,#13298,
#13299));
#13756=CLOSED_SHELL('',(#13300));
#13757=CLOSED_SHELL('',(#13301));
#13758=CLOSED_SHELL('',(#13302));
#13759=CLOSED_SHELL('',(#13303));
#13760=CLOSED_SHELL('',(#13304));
#13761=CLOSED_SHELL('',(#13305));
#13762=CLOSED_SHELL('',(#13306));
#13763=CLOSED_SHELL('',(#13307,#13308,#13309,#13310,#13311,#13312,#13313,
#13314,#13315,#13316,#13317,#13318,#13319,#13320,#13321,#13322,#13323));
#13764=CLOSED_SHELL('',(#13324,#13325,#13326,#13327));
#13765=CLOSED_SHELL('',(#13328,#13329,#13330,#13331));
#13766=CLOSED_SHELL('',(#13332,#13333,#13334,#13335,#13336,#13337,#13338,
#13339,#13340));
#13767=CLOSED_SHELL('',(#13341,#13342,#13343,#13344,#13345,#13346,#13347,
#13348));
#13768=CLOSED_SHELL('',(#13349,#13350,#13351,#13352,#13353,#13354,#13355,
#13356,#13357,#13358,#13359,#13360,#13361,#13362,#13363,#13364,#13365,#13366,
#13367,#13368,#13369,#13370,#13371,#13372,#13373));
#13769=CLOSED_SHELL('',(#13374,#13375,#13376,#13377));
#13770=CLOSED_SHELL('',(#13378,#13379,#13380,#13381,#13382,#13383,#13384,
#13385,#13386,#13387,#13388,#13389));
#13771=CLOSED_SHELL('',(#13390,#13391,#13392,#13393));
#13772=CLOSED_SHELL('',(#13394,#13395,#13396,#13397,#13398,#13399,#13400,
#13401));
#13773=CLOSED_SHELL('',(#13402,#13403,#13404,#13405,#13406,#13407,#13408,
#13409));
#13774=CLOSED_SHELL('',(#13410,#13411,#13412,#13413,#13414,#13415,#13416,
#13417));
#13775=CLOSED_SHELL('',(#13418,#13419,#13420,#13421,#13422,#13423,#13424,
#13425));
#13776=CLOSED_SHELL('',(#13426,#13427,#13428,#13429,#13430,#13431,#13432,
#13433,#13434,#13435,#13436));
#13777=CLOSED_SHELL('',(#13437,#13438,#13439,#13440,#13441,#13442));
#13778=CLOSED_SHELL('',(#13443,#13444,#13445,#13446));
#13779=CLOSED_SHELL('',(#13447,#13448,#13449));
#13780=CLOSED_SHELL('',(#13450,#13451,#13452));
#13781=CLOSED_SHELL('',(#13453,#13454,#13455,#13456));
#13782=CLOSED_SHELL('',(#13457,#13458,#13459));
#13783=CLOSED_SHELL('',(#13460,#13461,#13462,#13463,#13464,#13465,#13466,
#13467,#13468,#13469));
#13784=CLOSED_SHELL('',(#13470,#13471,#13472,#13473,#13474,#13475,#13476,
#13477,#13478,#13479,#13480,#13481,#13482,#13483,#13484,#13485,#13486,#13487,
#13488,#13489,#13490,#13491,#13492,#13493,#13494,#13495,#13496,#13497,#13498,
#13499,#13500,#13501,#13502,#13503,#13504,#13505,#13506,#13507,#13508,#13509,
#13510,#13511,#13512,#13513,#13514,#13515,#13516,#13517,#13518,#13519,#13520,
#13521,#13522));
#13785=CLOSED_SHELL('',(#13523,#13524,#13525,#13526,#13527,#13528,#13529,
#13530,#13531));
#13786=CLOSED_SHELL('',(#13532,#13533,#13534,#13535));
#13787=CLOSED_SHELL('',(#13536,#13537,#13538,#13539));
#13788=CLOSED_SHELL('',(#13540,#13541,#13542));
#13789=CLOSED_SHELL('',(#13543,#13544,#13545));
#13790=CLOSED_SHELL('',(#13546,#13547,#13548,#13549));
#13791=CLOSED_SHELL('',(#13550,#13551,#13552,#13553,#13554,#13555,#13556));
#13792=CLOSED_SHELL('',(#13557,#13558,#13559,#13560,#13561,#13562,#13563));
#13793=CLOSED_SHELL('',(#13564,#13565,#13566,#13567));
#13794=CLOSED_SHELL('',(#13568,#13569,#13570,#13571));
#13795=CLOSED_SHELL('',(#13572,#13573,#13574,#13575));
#13796=CLOSED_SHELL('',(#13576,#13577,#13578,#13579,#13580,#13581,#13582));
#13797=CLOSED_SHELL('',(#13583,#13584,#13585,#13586,#13587,#13588,#13589));
#13798=CLOSED_SHELL('',(#13590,#13591,#13592,#13593,#13594,#13595,#13596,
#13597,#13598,#13599,#13600,#13601,#13602,#13603,#13604,#13605,#13606,#13607,
#13608,#13609,#13610,#13611,#13612,#13613,#13614,#13615,#13616,#13617,#13618,
#13619,#13620,#13621,#13622,#13623,#13624,#13625,#13626,#13627,#13628,#13629,
#13630,#13631,#13632,#13633,#13634,#13635,#13636,#13637,#13638,#13639,#13640,
#13641,#13642,#13643,#13644,#13645,#13646,#13647,#13648,#13649,#13650,#13651,
#13652,#13653,#13654,#13655,#13656,#13657,#13658,#13659,#13660,#13661,#13662,
#13663,#13664,#13665,#13666,#13667,#13668,#13669,#13670,#13671,#13672,#13673,
#13674,#13675,#13676,#13677,#13678,#13679,#13680,#13681,#13682));
#13799=CLOSED_SHELL('',(#13683,#13684,#13685,#13686,#13687,#13688,#13689,
#13690,#13691));
#13800=CLOSED_SHELL('',(#13692,#13693,#13694,#13695,#13696,#13697,#13698,
#13699));
#13801=CLOSED_SHELL('',(#13700,#13701,#13702,#13703,#13704,#13705,#13706,
#13707,#13708,#13709,#13710,#13711));
#13802=DERIVED_UNIT_ELEMENT(#13940,1.);
#13803=DERIVED_UNIT_ELEMENT(#27071,-3.);
#13804=DERIVED_UNIT_ELEMENT(#13940,1.);
#13805=DERIVED_UNIT_ELEMENT(#27071,-3.);
#13806=DERIVED_UNIT_ELEMENT(#13940,1.);
#13807=DERIVED_UNIT_ELEMENT(#27071,-3.);
#13808=DERIVED_UNIT_ELEMENT(#13940,1.);
#13809=DERIVED_UNIT_ELEMENT(#27071,-3.);
#13810=DERIVED_UNIT_ELEMENT(#13940,1.);
#13811=DERIVED_UNIT_ELEMENT(#27071,-3.);
#13812=DERIVED_UNIT_ELEMENT(#13940,1.);
#13813=DERIVED_UNIT_ELEMENT(#27071,-3.);
#13814=DERIVED_UNIT_ELEMENT(#13940,1.);
#13815=DERIVED_UNIT_ELEMENT(#27071,-3.);
#13816=DERIVED_UNIT_ELEMENT(#13940,1.);
#13817=DERIVED_UNIT_ELEMENT(#27071,-3.);
#13818=DERIVED_UNIT_ELEMENT(#13940,1.);
#13819=DERIVED_UNIT_ELEMENT(#27071,-3.);
#13820=DERIVED_UNIT_ELEMENT(#13940,1.);
#13821=DERIVED_UNIT_ELEMENT(#27071,-3.);
#13822=DERIVED_UNIT_ELEMENT(#13940,1.);
#13823=DERIVED_UNIT_ELEMENT(#27071,-3.);
#13824=DERIVED_UNIT_ELEMENT(#13940,1.);
#13825=DERIVED_UNIT_ELEMENT(#27071,-3.);
#13826=DERIVED_UNIT_ELEMENT(#13940,1.);
#13827=DERIVED_UNIT_ELEMENT(#27071,-3.);
#13828=DERIVED_UNIT_ELEMENT(#13940,1.);
#13829=DERIVED_UNIT_ELEMENT(#27071,-3.);
#13830=DERIVED_UNIT_ELEMENT(#13940,1.);
#13831=DERIVED_UNIT_ELEMENT(#27071,-3.);
#13832=DERIVED_UNIT_ELEMENT(#13940,1.);
#13833=DERIVED_UNIT_ELEMENT(#27071,-3.);
#13834=DERIVED_UNIT_ELEMENT(#13940,1.);
#13835=DERIVED_UNIT_ELEMENT(#27071,-3.);
#13836=DERIVED_UNIT_ELEMENT(#13940,1.);
#13837=DERIVED_UNIT_ELEMENT(#27071,-3.);
#13838=DERIVED_UNIT_ELEMENT(#13940,1.);
#13839=DERIVED_UNIT_ELEMENT(#27071,-3.);
#13840=DERIVED_UNIT_ELEMENT(#13940,1.);
#13841=DERIVED_UNIT_ELEMENT(#27071,-3.);
#13842=DERIVED_UNIT_ELEMENT(#13940,1.);
#13843=DERIVED_UNIT_ELEMENT(#27071,-3.);
#13844=DERIVED_UNIT_ELEMENT(#13940,1.);
#13845=DERIVED_UNIT_ELEMENT(#27071,-3.);
#13846=DERIVED_UNIT_ELEMENT(#13940,1.);
#13847=DERIVED_UNIT_ELEMENT(#27071,-3.);
#13848=DERIVED_UNIT_ELEMENT(#13940,1.);
#13849=DERIVED_UNIT_ELEMENT(#27071,-3.);
#13850=DERIVED_UNIT_ELEMENT(#13940,1.);
#13851=DERIVED_UNIT_ELEMENT(#27071,-3.);
#13852=DERIVED_UNIT_ELEMENT(#13940,1.);
#13853=DERIVED_UNIT_ELEMENT(#27071,-3.);
#13854=DERIVED_UNIT_ELEMENT(#13940,1.);
#13855=DERIVED_UNIT_ELEMENT(#27071,-3.);
#13856=DERIVED_UNIT_ELEMENT(#13940,1.);
#13857=DERIVED_UNIT_ELEMENT(#27071,-3.);
#13858=DERIVED_UNIT_ELEMENT(#13940,1.);
#13859=DERIVED_UNIT_ELEMENT(#27071,-3.);
#13860=DERIVED_UNIT_ELEMENT(#13940,1.);
#13861=DERIVED_UNIT_ELEMENT(#27071,-3.);
#13862=DERIVED_UNIT_ELEMENT(#13940,1.);
#13863=DERIVED_UNIT_ELEMENT(#27071,-3.);
#13864=DERIVED_UNIT_ELEMENT(#13940,1.);
#13865=DERIVED_UNIT_ELEMENT(#27071,-3.);
#13866=DERIVED_UNIT_ELEMENT(#13940,1.);
#13867=DERIVED_UNIT_ELEMENT(#27071,-3.);
#13868=DERIVED_UNIT_ELEMENT(#13940,1.);
#13869=DERIVED_UNIT_ELEMENT(#27071,-3.);
#13870=DERIVED_UNIT_ELEMENT(#13940,1.);
#13871=DERIVED_UNIT_ELEMENT(#27071,-3.);
#13872=DERIVED_UNIT_ELEMENT(#13940,1.);
#13873=DERIVED_UNIT_ELEMENT(#27071,-3.);
#13874=DERIVED_UNIT_ELEMENT(#13940,1.);
#13875=DERIVED_UNIT_ELEMENT(#27071,-3.);
#13876=DERIVED_UNIT_ELEMENT(#13940,1.);
#13877=DERIVED_UNIT_ELEMENT(#27071,-3.);
#13878=DERIVED_UNIT_ELEMENT(#13940,1.);
#13879=DERIVED_UNIT_ELEMENT(#27071,-3.);
#13880=DERIVED_UNIT_ELEMENT(#13940,1.);
#13881=DERIVED_UNIT_ELEMENT(#27071,-3.);
#13882=DERIVED_UNIT_ELEMENT(#13940,1.);
#13883=DERIVED_UNIT_ELEMENT(#27071,-3.);
#13884=DERIVED_UNIT_ELEMENT(#13940,1.);
#13885=DERIVED_UNIT_ELEMENT(#27071,-3.);
#13886=DERIVED_UNIT_ELEMENT(#13940,1.);
#13887=DERIVED_UNIT_ELEMENT(#27071,-3.);
#13888=DERIVED_UNIT_ELEMENT(#13940,1.);
#13889=DERIVED_UNIT_ELEMENT(#27071,-3.);
#13890=DERIVED_UNIT_ELEMENT(#13940,1.);
#13891=DERIVED_UNIT_ELEMENT(#27071,-3.);
#13892=DERIVED_UNIT_ELEMENT(#13940,1.);
#13893=DERIVED_UNIT_ELEMENT(#27071,-3.);
#13894=DERIVED_UNIT_ELEMENT(#13940,1.);
#13895=DERIVED_UNIT_ELEMENT(#27071,-3.);
#13896=DERIVED_UNIT_ELEMENT(#13940,1.);
#13897=DERIVED_UNIT_ELEMENT(#27071,-3.);
#13898=DERIVED_UNIT_ELEMENT(#13940,1.);
#13899=DERIVED_UNIT_ELEMENT(#27071,-3.);
#13900=DERIVED_UNIT_ELEMENT(#13940,1.);
#13901=DERIVED_UNIT_ELEMENT(#27071,-3.);
#13902=DERIVED_UNIT_ELEMENT(#13940,1.);
#13903=DERIVED_UNIT_ELEMENT(#27071,-3.);
#13904=DERIVED_UNIT_ELEMENT(#13940,1.);
#13905=DERIVED_UNIT_ELEMENT(#27071,-3.);
#13906=DERIVED_UNIT_ELEMENT(#13940,1.);
#13907=DERIVED_UNIT_ELEMENT(#27071,-3.);
#13908=DERIVED_UNIT_ELEMENT(#13940,1.);
#13909=DERIVED_UNIT_ELEMENT(#27071,-3.);
#13910=DERIVED_UNIT_ELEMENT(#13940,1.);
#13911=DERIVED_UNIT_ELEMENT(#27071,-3.);
#13912=DERIVED_UNIT_ELEMENT(#13940,1.);
#13913=DERIVED_UNIT_ELEMENT(#27071,-3.);
#13914=DERIVED_UNIT_ELEMENT(#13940,1.);
#13915=DERIVED_UNIT_ELEMENT(#27071,-3.);
#13916=DERIVED_UNIT_ELEMENT(#13940,1.);
#13917=DERIVED_UNIT_ELEMENT(#27071,-3.);
#13918=DERIVED_UNIT_ELEMENT(#13940,1.);
#13919=DERIVED_UNIT_ELEMENT(#27071,-3.);
#13920=DERIVED_UNIT_ELEMENT(#13940,1.);
#13921=DERIVED_UNIT_ELEMENT(#27071,-3.);
#13922=DERIVED_UNIT_ELEMENT(#13940,1.);
#13923=DERIVED_UNIT_ELEMENT(#27071,-3.);
#13924=DERIVED_UNIT_ELEMENT(#13940,1.);
#13925=DERIVED_UNIT_ELEMENT(#27071,-3.);
#13926=DERIVED_UNIT_ELEMENT(#13940,1.);
#13927=DERIVED_UNIT_ELEMENT(#27071,-3.);
#13928=DERIVED_UNIT_ELEMENT(#13940,1.);
#13929=DERIVED_UNIT_ELEMENT(#27071,-3.);
#13930=DERIVED_UNIT_ELEMENT(#13940,1.);
#13931=DERIVED_UNIT_ELEMENT(#27071,-3.);
#13932=DERIVED_UNIT_ELEMENT(#13940,1.);
#13933=DERIVED_UNIT_ELEMENT(#27071,-3.);
#13934=DERIVED_UNIT_ELEMENT(#13940,1.);
#13935=DERIVED_UNIT_ELEMENT(#27071,-3.);
#13936=DERIVED_UNIT_ELEMENT(#13940,1.);
#13937=DERIVED_UNIT_ELEMENT(#27071,-3.);
#13938=DERIVED_UNIT_ELEMENT(#13940,1.);
#13939=DERIVED_UNIT_ELEMENT(#27071,-3.);
#13940=(
MASS_UNIT()
NAMED_UNIT(*)
SI_UNIT(.KILO.,.GRAM.)
);
#13941=DERIVED_UNIT((#13802,#13803));
#13942=DERIVED_UNIT((#13804,#13805));
#13943=DERIVED_UNIT((#13806,#13807));
#13944=DERIVED_UNIT((#13808,#13809));
#13945=DERIVED_UNIT((#13810,#13811));
#13946=DERIVED_UNIT((#13812,#13813));
#13947=DERIVED_UNIT((#13814,#13815));
#13948=DERIVED_UNIT((#13816,#13817));
#13949=DERIVED_UNIT((#13818,#13819));
#13950=DERIVED_UNIT((#13820,#13821));
#13951=DERIVED_UNIT((#13822,#13823));
#13952=DERIVED_UNIT((#13824,#13825));
#13953=DERIVED_UNIT((#13826,#13827));
#13954=DERIVED_UNIT((#13828,#13829));
#13955=DERIVED_UNIT((#13830,#13831));
#13956=DERIVED_UNIT((#13832,#13833));
#13957=DERIVED_UNIT((#13834,#13835));
#13958=DERIVED_UNIT((#13836,#13837));
#13959=DERIVED_UNIT((#13838,#13839));
#13960=DERIVED_UNIT((#13840,#13841));
#13961=DERIVED_UNIT((#13842,#13843));
#13962=DERIVED_UNIT((#13844,#13845));
#13963=DERIVED_UNIT((#13846,#13847));
#13964=DERIVED_UNIT((#13848,#13849));
#13965=DERIVED_UNIT((#13850,#13851));
#13966=DERIVED_UNIT((#13852,#13853));
#13967=DERIVED_UNIT((#13854,#13855));
#13968=DERIVED_UNIT((#13856,#13857));
#13969=DERIVED_UNIT((#13858,#13859));
#13970=DERIVED_UNIT((#13860,#13861));
#13971=DERIVED_UNIT((#13862,#13863));
#13972=DERIVED_UNIT((#13864,#13865));
#13973=DERIVED_UNIT((#13866,#13867));
#13974=DERIVED_UNIT((#13868,#13869));
#13975=DERIVED_UNIT((#13870,#13871));
#13976=DERIVED_UNIT((#13872,#13873));
#13977=DERIVED_UNIT((#13874,#13875));
#13978=DERIVED_UNIT((#13876,#13877));
#13979=DERIVED_UNIT((#13878,#13879));
#13980=DERIVED_UNIT((#13880,#13881));
#13981=DERIVED_UNIT((#13882,#13883));
#13982=DERIVED_UNIT((#13884,#13885));
#13983=DERIVED_UNIT((#13886,#13887));
#13984=DERIVED_UNIT((#13888,#13889));
#13985=DERIVED_UNIT((#13890,#13891));
#13986=DERIVED_UNIT((#13892,#13893));
#13987=DERIVED_UNIT((#13894,#13895));
#13988=DERIVED_UNIT((#13896,#13897));
#13989=DERIVED_UNIT((#13898,#13899));
#13990=DERIVED_UNIT((#13900,#13901));
#13991=DERIVED_UNIT((#13902,#13903));
#13992=DERIVED_UNIT((#13904,#13905));
#13993=DERIVED_UNIT((#13906,#13907));
#13994=DERIVED_UNIT((#13908,#13909));
#13995=DERIVED_UNIT((#13910,#13911));
#13996=DERIVED_UNIT((#13912,#13913));
#13997=DERIVED_UNIT((#13914,#13915));
#13998=DERIVED_UNIT((#13916,#13917));
#13999=DERIVED_UNIT((#13918,#13919));
#14000=DERIVED_UNIT((#13920,#13921));
#14001=DERIVED_UNIT((#13922,#13923));
#14002=DERIVED_UNIT((#13924,#13925));
#14003=DERIVED_UNIT((#13926,#13927));
#14004=DERIVED_UNIT((#13928,#13929));
#14005=DERIVED_UNIT((#13930,#13931));
#14006=DERIVED_UNIT((#13932,#13933));
#14007=DERIVED_UNIT((#13934,#13935));
#14008=DERIVED_UNIT((#13936,#13937));
#14009=DERIVED_UNIT((#13938,#13939));
#14010=MEASURE_REPRESENTATION_ITEM('density measure',
POSITIVE_RATIO_MEASURE(7850.),#13941);
#14011=MEASURE_REPRESENTATION_ITEM('density measure',
POSITIVE_RATIO_MEASURE(7850.),#13942);
#14012=MEASURE_REPRESENTATION_ITEM('density measure',
POSITIVE_RATIO_MEASURE(7850.),#13943);
#14013=MEASURE_REPRESENTATION_ITEM('density measure',
POSITIVE_RATIO_MEASURE(7850.),#13944);
#14014=MEASURE_REPRESENTATION_ITEM('density measure',
POSITIVE_RATIO_MEASURE(7850.),#13945);
#14015=MEASURE_REPRESENTATION_ITEM('density measure',
POSITIVE_RATIO_MEASURE(7850.),#13946);
#14016=MEASURE_REPRESENTATION_ITEM('density measure',
POSITIVE_RATIO_MEASURE(7850.),#13947);
#14017=MEASURE_REPRESENTATION_ITEM('density measure',
POSITIVE_RATIO_MEASURE(7850.),#13948);
#14018=MEASURE_REPRESENTATION_ITEM('density measure',
POSITIVE_RATIO_MEASURE(7850.),#13949);
#14019=MEASURE_REPRESENTATION_ITEM('density measure',
POSITIVE_RATIO_MEASURE(7850.),#13950);
#14020=MEASURE_REPRESENTATION_ITEM('density measure',
POSITIVE_RATIO_MEASURE(7850.),#13951);
#14021=MEASURE_REPRESENTATION_ITEM('density measure',
POSITIVE_RATIO_MEASURE(7850.),#13952);
#14022=MEASURE_REPRESENTATION_ITEM('density measure',
POSITIVE_RATIO_MEASURE(7850.),#13953);
#14023=MEASURE_REPRESENTATION_ITEM('density measure',
POSITIVE_RATIO_MEASURE(7850.),#13954);
#14024=MEASURE_REPRESENTATION_ITEM('density measure',
POSITIVE_RATIO_MEASURE(7850.),#13955);
#14025=MEASURE_REPRESENTATION_ITEM('density measure',
POSITIVE_RATIO_MEASURE(7850.),#13956);
#14026=MEASURE_REPRESENTATION_ITEM('density measure',
POSITIVE_RATIO_MEASURE(7850.),#13957);
#14027=MEASURE_REPRESENTATION_ITEM('density measure',
POSITIVE_RATIO_MEASURE(7850.),#13958);
#14028=MEASURE_REPRESENTATION_ITEM('density measure',
POSITIVE_RATIO_MEASURE(7850.),#13959);
#14029=MEASURE_REPRESENTATION_ITEM('density measure',
POSITIVE_RATIO_MEASURE(7850.),#13960);
#14030=MEASURE_REPRESENTATION_ITEM('density measure',
POSITIVE_RATIO_MEASURE(7850.),#13961);
#14031=MEASURE_REPRESENTATION_ITEM('density measure',
POSITIVE_RATIO_MEASURE(7850.),#13962);
#14032=MEASURE_REPRESENTATION_ITEM('density measure',
POSITIVE_RATIO_MEASURE(7850.),#13963);
#14033=MEASURE_REPRESENTATION_ITEM('density measure',
POSITIVE_RATIO_MEASURE(7850.),#13964);
#14034=MEASURE_REPRESENTATION_ITEM('density measure',
POSITIVE_RATIO_MEASURE(7850.),#13965);
#14035=MEASURE_REPRESENTATION_ITEM('density measure',
POSITIVE_RATIO_MEASURE(7850.),#13966);
#14036=MEASURE_REPRESENTATION_ITEM('density measure',
POSITIVE_RATIO_MEASURE(7850.),#13967);
#14037=MEASURE_REPRESENTATION_ITEM('density measure',
POSITIVE_RATIO_MEASURE(7850.),#13968);
#14038=MEASURE_REPRESENTATION_ITEM('density measure',
POSITIVE_RATIO_MEASURE(7850.),#13969);
#14039=MEASURE_REPRESENTATION_ITEM('density measure',
POSITIVE_RATIO_MEASURE(7850.),#13970);
#14040=MEASURE_REPRESENTATION_ITEM('density measure',
POSITIVE_RATIO_MEASURE(7850.),#13971);
#14041=MEASURE_REPRESENTATION_ITEM('density measure',
POSITIVE_RATIO_MEASURE(7850.),#13972);
#14042=MEASURE_REPRESENTATION_ITEM('density measure',
POSITIVE_RATIO_MEASURE(7850.),#13973);
#14043=MEASURE_REPRESENTATION_ITEM('density measure',
POSITIVE_RATIO_MEASURE(7850.),#13974);
#14044=MEASURE_REPRESENTATION_ITEM('density measure',
POSITIVE_RATIO_MEASURE(7850.),#13975);
#14045=MEASURE_REPRESENTATION_ITEM('density measure',
POSITIVE_RATIO_MEASURE(7850.),#13976);
#14046=MEASURE_REPRESENTATION_ITEM('density measure',
POSITIVE_RATIO_MEASURE(7850.),#13977);
#14047=MEASURE_REPRESENTATION_ITEM('density measure',
POSITIVE_RATIO_MEASURE(7850.),#13978);
#14048=MEASURE_REPRESENTATION_ITEM('density measure',
POSITIVE_RATIO_MEASURE(7850.),#13979);
#14049=MEASURE_REPRESENTATION_ITEM('density measure',
POSITIVE_RATIO_MEASURE(7850.),#13980);
#14050=MEASURE_REPRESENTATION_ITEM('density measure',
POSITIVE_RATIO_MEASURE(7850.),#13981);
#14051=MEASURE_REPRESENTATION_ITEM('density measure',
POSITIVE_RATIO_MEASURE(7850.),#13982);
#14052=MEASURE_REPRESENTATION_ITEM('density measure',
POSITIVE_RATIO_MEASURE(7850.),#13983);
#14053=MEASURE_REPRESENTATION_ITEM('density measure',
POSITIVE_RATIO_MEASURE(7850.),#13984);
#14054=MEASURE_REPRESENTATION_ITEM('density measure',
POSITIVE_RATIO_MEASURE(7850.),#13985);
#14055=MEASURE_REPRESENTATION_ITEM('density measure',
POSITIVE_RATIO_MEASURE(7850.),#13986);
#14056=MEASURE_REPRESENTATION_ITEM('density measure',
POSITIVE_RATIO_MEASURE(7850.),#13987);
#14057=MEASURE_REPRESENTATION_ITEM('density measure',
POSITIVE_RATIO_MEASURE(7850.),#13988);
#14058=MEASURE_REPRESENTATION_ITEM('density measure',
POSITIVE_RATIO_MEASURE(7850.),#13989);
#14059=MEASURE_REPRESENTATION_ITEM('density measure',
POSITIVE_RATIO_MEASURE(7850.),#13990);
#14060=MEASURE_REPRESENTATION_ITEM('density measure',
POSITIVE_RATIO_MEASURE(7850.),#13991);
#14061=MEASURE_REPRESENTATION_ITEM('density measure',
POSITIVE_RATIO_MEASURE(7850.),#13992);
#14062=MEASURE_REPRESENTATION_ITEM('density measure',
POSITIVE_RATIO_MEASURE(7850.),#13993);
#14063=MEASURE_REPRESENTATION_ITEM('density measure',
POSITIVE_RATIO_MEASURE(7850.),#13994);
#14064=MEASURE_REPRESENTATION_ITEM('density measure',
POSITIVE_RATIO_MEASURE(7850.),#13995);
#14065=MEASURE_REPRESENTATION_ITEM('density measure',
POSITIVE_RATIO_MEASURE(7850.),#13996);
#14066=MEASURE_REPRESENTATION_ITEM('density measure',
POSITIVE_RATIO_MEASURE(7850.),#13997);
#14067=MEASURE_REPRESENTATION_ITEM('density measure',
POSITIVE_RATIO_MEASURE(7850.),#13998);
#14068=MEASURE_REPRESENTATION_ITEM('density measure',
POSITIVE_RATIO_MEASURE(7850.),#13999);
#14069=MEASURE_REPRESENTATION_ITEM('density measure',
POSITIVE_RATIO_MEASURE(7850.),#14000);
#14070=MEASURE_REPRESENTATION_ITEM('density measure',
POSITIVE_RATIO_MEASURE(7850.),#14001);
#14071=MEASURE_REPRESENTATION_ITEM('density measure',
POSITIVE_RATIO_MEASURE(7850.),#14002);
#14072=MEASURE_REPRESENTATION_ITEM('density measure',
POSITIVE_RATIO_MEASURE(7850.),#14003);
#14073=MEASURE_REPRESENTATION_ITEM('density measure',
POSITIVE_RATIO_MEASURE(7850.),#14004);
#14074=MEASURE_REPRESENTATION_ITEM('density measure',
POSITIVE_RATIO_MEASURE(7850.),#14005);
#14075=MEASURE_REPRESENTATION_ITEM('density measure',
POSITIVE_RATIO_MEASURE(7850.),#14006);
#14076=MEASURE_REPRESENTATION_ITEM('density measure',
POSITIVE_RATIO_MEASURE(7850.),#14007);
#14077=MEASURE_REPRESENTATION_ITEM('density measure',
POSITIVE_RATIO_MEASURE(7850.),#14008);
#14078=MEASURE_REPRESENTATION_ITEM('density measure',
POSITIVE_RATIO_MEASURE(7850.),#14009);
#14079=PROPERTY_DEFINITION_REPRESENTATION(#14424,#14217);
#14080=PROPERTY_DEFINITION_REPRESENTATION(#14425,#14218);
#14081=PROPERTY_DEFINITION_REPRESENTATION(#14426,#14219);
#14082=PROPERTY_DEFINITION_REPRESENTATION(#14427,#14220);
#14083=PROPERTY_DEFINITION_REPRESENTATION(#14428,#14221);
#14084=PROPERTY_DEFINITION_REPRESENTATION(#14429,#14222);
#14085=PROPERTY_DEFINITION_REPRESENTATION(#14430,#14223);
#14086=PROPERTY_DEFINITION_REPRESENTATION(#14431,#14224);
#14087=PROPERTY_DEFINITION_REPRESENTATION(#14432,#14225);
#14088=PROPERTY_DEFINITION_REPRESENTATION(#14433,#14226);
#14089=PROPERTY_DEFINITION_REPRESENTATION(#14434,#14227);
#14090=PROPERTY_DEFINITION_REPRESENTATION(#14435,#14228);
#14091=PROPERTY_DEFINITION_REPRESENTATION(#14436,#14229);
#14092=PROPERTY_DEFINITION_REPRESENTATION(#14437,#14230);
#14093=PROPERTY_DEFINITION_REPRESENTATION(#14438,#14231);
#14094=PROPERTY_DEFINITION_REPRESENTATION(#14439,#14232);
#14095=PROPERTY_DEFINITION_REPRESENTATION(#14440,#14233);
#14096=PROPERTY_DEFINITION_REPRESENTATION(#14441,#14234);
#14097=PROPERTY_DEFINITION_REPRESENTATION(#14442,#14235);
#14098=PROPERTY_DEFINITION_REPRESENTATION(#14443,#14236);
#14099=PROPERTY_DEFINITION_REPRESENTATION(#14444,#14237);
#14100=PROPERTY_DEFINITION_REPRESENTATION(#14445,#14238);
#14101=PROPERTY_DEFINITION_REPRESENTATION(#14446,#14239);
#14102=PROPERTY_DEFINITION_REPRESENTATION(#14447,#14240);
#14103=PROPERTY_DEFINITION_REPRESENTATION(#14448,#14241);
#14104=PROPERTY_DEFINITION_REPRESENTATION(#14449,#14242);
#14105=PROPERTY_DEFINITION_REPRESENTATION(#14450,#14243);
#14106=PROPERTY_DEFINITION_REPRESENTATION(#14451,#14244);
#14107=PROPERTY_DEFINITION_REPRESENTATION(#14452,#14245);
#14108=PROPERTY_DEFINITION_REPRESENTATION(#14453,#14246);
#14109=PROPERTY_DEFINITION_REPRESENTATION(#14454,#14247);
#14110=PROPERTY_DEFINITION_REPRESENTATION(#14455,#14248);
#14111=PROPERTY_DEFINITION_REPRESENTATION(#14456,#14249);
#14112=PROPERTY_DEFINITION_REPRESENTATION(#14457,#14250);
#14113=PROPERTY_DEFINITION_REPRESENTATION(#14458,#14251);
#14114=PROPERTY_DEFINITION_REPRESENTATION(#14459,#14252);
#14115=PROPERTY_DEFINITION_REPRESENTATION(#14460,#14253);
#14116=PROPERTY_DEFINITION_REPRESENTATION(#14461,#14254);
#14117=PROPERTY_DEFINITION_REPRESENTATION(#14462,#14255);
#14118=PROPERTY_DEFINITION_REPRESENTATION(#14463,#14256);
#14119=PROPERTY_DEFINITION_REPRESENTATION(#14464,#14257);
#14120=PROPERTY_DEFINITION_REPRESENTATION(#14465,#14258);
#14121=PROPERTY_DEFINITION_REPRESENTATION(#14466,#14259);
#14122=PROPERTY_DEFINITION_REPRESENTATION(#14467,#14260);
#14123=PROPERTY_DEFINITION_REPRESENTATION(#14468,#14261);
#14124=PROPERTY_DEFINITION_REPRESENTATION(#14469,#14262);
#14125=PROPERTY_DEFINITION_REPRESENTATION(#14470,#14263);
#14126=PROPERTY_DEFINITION_REPRESENTATION(#14471,#14264);
#14127=PROPERTY_DEFINITION_REPRESENTATION(#14472,#14265);
#14128=PROPERTY_DEFINITION_REPRESENTATION(#14473,#14266);
#14129=PROPERTY_DEFINITION_REPRESENTATION(#14474,#14267);
#14130=PROPERTY_DEFINITION_REPRESENTATION(#14475,#14268);
#14131=PROPERTY_DEFINITION_REPRESENTATION(#14476,#14269);
#14132=PROPERTY_DEFINITION_REPRESENTATION(#14477,#14270);
#14133=PROPERTY_DEFINITION_REPRESENTATION(#14478,#14271);
#14134=PROPERTY_DEFINITION_REPRESENTATION(#14479,#14272);
#14135=PROPERTY_DEFINITION_REPRESENTATION(#14480,#14273);
#14136=PROPERTY_DEFINITION_REPRESENTATION(#14481,#14274);
#14137=PROPERTY_DEFINITION_REPRESENTATION(#14482,#14275);
#14138=PROPERTY_DEFINITION_REPRESENTATION(#14483,#14276);
#14139=PROPERTY_DEFINITION_REPRESENTATION(#14484,#14277);
#14140=PROPERTY_DEFINITION_REPRESENTATION(#14485,#14278);
#14141=PROPERTY_DEFINITION_REPRESENTATION(#14486,#14279);
#14142=PROPERTY_DEFINITION_REPRESENTATION(#14487,#14280);
#14143=PROPERTY_DEFINITION_REPRESENTATION(#14488,#14281);
#14144=PROPERTY_DEFINITION_REPRESENTATION(#14489,#14282);
#14145=PROPERTY_DEFINITION_REPRESENTATION(#14490,#14283);
#14146=PROPERTY_DEFINITION_REPRESENTATION(#14491,#14284);
#14147=PROPERTY_DEFINITION_REPRESENTATION(#14492,#14285);
#14148=PROPERTY_DEFINITION_REPRESENTATION(#14493,#14286);
#14149=PROPERTY_DEFINITION_REPRESENTATION(#14494,#14287);
#14150=PROPERTY_DEFINITION_REPRESENTATION(#14495,#14288);
#14151=PROPERTY_DEFINITION_REPRESENTATION(#14496,#14289);
#14152=PROPERTY_DEFINITION_REPRESENTATION(#14497,#14290);
#14153=PROPERTY_DEFINITION_REPRESENTATION(#14498,#14291);
#14154=PROPERTY_DEFINITION_REPRESENTATION(#14499,#14292);
#14155=PROPERTY_DEFINITION_REPRESENTATION(#14500,#14293);
#14156=PROPERTY_DEFINITION_REPRESENTATION(#14501,#14294);
#14157=PROPERTY_DEFINITION_REPRESENTATION(#14502,#14295);
#14158=PROPERTY_DEFINITION_REPRESENTATION(#14503,#14296);
#14159=PROPERTY_DEFINITION_REPRESENTATION(#14504,#14297);
#14160=PROPERTY_DEFINITION_REPRESENTATION(#14505,#14298);
#14161=PROPERTY_DEFINITION_REPRESENTATION(#14506,#14299);
#14162=PROPERTY_DEFINITION_REPRESENTATION(#14507,#14300);
#14163=PROPERTY_DEFINITION_REPRESENTATION(#14508,#14301);
#14164=PROPERTY_DEFINITION_REPRESENTATION(#14509,#14302);
#14165=PROPERTY_DEFINITION_REPRESENTATION(#14510,#14303);
#14166=PROPERTY_DEFINITION_REPRESENTATION(#14511,#14304);
#14167=PROPERTY_DEFINITION_REPRESENTATION(#14512,#14305);
#14168=PROPERTY_DEFINITION_REPRESENTATION(#14513,#14306);
#14169=PROPERTY_DEFINITION_REPRESENTATION(#14514,#14307);
#14170=PROPERTY_DEFINITION_REPRESENTATION(#14515,#14308);
#14171=PROPERTY_DEFINITION_REPRESENTATION(#14516,#14309);
#14172=PROPERTY_DEFINITION_REPRESENTATION(#14517,#14310);
#14173=PROPERTY_DEFINITION_REPRESENTATION(#14518,#14311);
#14174=PROPERTY_DEFINITION_REPRESENTATION(#14519,#14312);
#14175=PROPERTY_DEFINITION_REPRESENTATION(#14520,#14313);
#14176=PROPERTY_DEFINITION_REPRESENTATION(#14521,#14314);
#14177=PROPERTY_DEFINITION_REPRESENTATION(#14522,#14315);
#14178=PROPERTY_DEFINITION_REPRESENTATION(#14523,#14316);
#14179=PROPERTY_DEFINITION_REPRESENTATION(#14524,#14317);
#14180=PROPERTY_DEFINITION_REPRESENTATION(#14525,#14318);
#14181=PROPERTY_DEFINITION_REPRESENTATION(#14526,#14319);
#14182=PROPERTY_DEFINITION_REPRESENTATION(#14527,#14320);
#14183=PROPERTY_DEFINITION_REPRESENTATION(#14528,#14321);
#14184=PROPERTY_DEFINITION_REPRESENTATION(#14529,#14322);
#14185=PROPERTY_DEFINITION_REPRESENTATION(#14530,#14323);
#14186=PROPERTY_DEFINITION_REPRESENTATION(#14531,#14324);
#14187=PROPERTY_DEFINITION_REPRESENTATION(#14532,#14325);
#14188=PROPERTY_DEFINITION_REPRESENTATION(#14533,#14326);
#14189=PROPERTY_DEFINITION_REPRESENTATION(#14534,#14327);
#14190=PROPERTY_DEFINITION_REPRESENTATION(#14535,#14328);
#14191=PROPERTY_DEFINITION_REPRESENTATION(#14536,#14329);
#14192=PROPERTY_DEFINITION_REPRESENTATION(#14537,#14330);
#14193=PROPERTY_DEFINITION_REPRESENTATION(#14538,#14331);
#14194=PROPERTY_DEFINITION_REPRESENTATION(#14539,#14332);
#14195=PROPERTY_DEFINITION_REPRESENTATION(#14540,#14333);
#14196=PROPERTY_DEFINITION_REPRESENTATION(#14541,#14334);
#14197=PROPERTY_DEFINITION_REPRESENTATION(#14542,#14335);
#14198=PROPERTY_DEFINITION_REPRESENTATION(#14543,#14336);
#14199=PROPERTY_DEFINITION_REPRESENTATION(#14544,#14337);
#14200=PROPERTY_DEFINITION_REPRESENTATION(#14545,#14338);
#14201=PROPERTY_DEFINITION_REPRESENTATION(#14546,#14339);
#14202=PROPERTY_DEFINITION_REPRESENTATION(#14547,#14340);
#14203=PROPERTY_DEFINITION_REPRESENTATION(#14548,#14341);
#14204=PROPERTY_DEFINITION_REPRESENTATION(#14549,#14342);
#14205=PROPERTY_DEFINITION_REPRESENTATION(#14550,#14343);
#14206=PROPERTY_DEFINITION_REPRESENTATION(#14551,#14344);
#14207=PROPERTY_DEFINITION_REPRESENTATION(#14552,#14345);
#14208=PROPERTY_DEFINITION_REPRESENTATION(#14553,#14346);
#14209=PROPERTY_DEFINITION_REPRESENTATION(#14554,#14347);
#14210=PROPERTY_DEFINITION_REPRESENTATION(#14555,#14348);
#14211=PROPERTY_DEFINITION_REPRESENTATION(#14556,#14349);
#14212=PROPERTY_DEFINITION_REPRESENTATION(#14557,#14350);
#14213=PROPERTY_DEFINITION_REPRESENTATION(#14558,#14351);
#14214=PROPERTY_DEFINITION_REPRESENTATION(#14559,#14352);
#14215=PROPERTY_DEFINITION_REPRESENTATION(#14560,#14353);
#14216=PROPERTY_DEFINITION_REPRESENTATION(#14561,#14354);
#14217=REPRESENTATION('material name',(#14355),#26995);
#14218=REPRESENTATION('density',(#14010),#26995);
#14219=REPRESENTATION('material name',(#14356),#26996);
#14220=REPRESENTATION('density',(#14011),#26996);
#14221=REPRESENTATION('material name',(#14357),#26997);
#14222=REPRESENTATION('density',(#14012),#26997);
#14223=REPRESENTATION('material name',(#14358),#26998);
#14224=REPRESENTATION('density',(#14013),#26998);
#14225=REPRESENTATION('material name',(#14359),#26999);
#14226=REPRESENTATION('density',(#14014),#26999);
#14227=REPRESENTATION('material name',(#14360),#27000);
#14228=REPRESENTATION('density',(#14015),#27000);
#14229=REPRESENTATION('material name',(#14361),#27001);
#14230=REPRESENTATION('density',(#14016),#27001);
#14231=REPRESENTATION('material name',(#14362),#27002);
#14232=REPRESENTATION('density',(#14017),#27002);
#14233=REPRESENTATION('material name',(#14363),#27003);
#14234=REPRESENTATION('density',(#14018),#27003);
#14235=REPRESENTATION('material name',(#14364),#27004);
#14236=REPRESENTATION('density',(#14019),#27004);
#14237=REPRESENTATION('material name',(#14365),#27005);
#14238=REPRESENTATION('density',(#14020),#27005);
#14239=REPRESENTATION('material name',(#14366),#27006);
#14240=REPRESENTATION('density',(#14021),#27006);
#14241=REPRESENTATION('material name',(#14367),#27007);
#14242=REPRESENTATION('density',(#14022),#27007);
#14243=REPRESENTATION('material name',(#14368),#27008);
#14244=REPRESENTATION('density',(#14023),#27008);
#14245=REPRESENTATION('material name',(#14369),#27009);
#14246=REPRESENTATION('density',(#14024),#27009);
#14247=REPRESENTATION('material name',(#14370),#27010);
#14248=REPRESENTATION('density',(#14025),#27010);
#14249=REPRESENTATION('material name',(#14371),#27011);
#14250=REPRESENTATION('density',(#14026),#27011);
#14251=REPRESENTATION('material name',(#14372),#27012);
#14252=REPRESENTATION('density',(#14027),#27012);
#14253=REPRESENTATION('material name',(#14373),#27013);
#14254=REPRESENTATION('density',(#14028),#27013);
#14255=REPRESENTATION('material name',(#14374),#27014);
#14256=REPRESENTATION('density',(#14029),#27014);
#14257=REPRESENTATION('material name',(#14375),#27015);
#14258=REPRESENTATION('density',(#14030),#27015);
#14259=REPRESENTATION('material name',(#14376),#27016);
#14260=REPRESENTATION('density',(#14031),#27016);
#14261=REPRESENTATION('material name',(#14377),#27017);
#14262=REPRESENTATION('density',(#14032),#27017);
#14263=REPRESENTATION('material name',(#14378),#27018);
#14264=REPRESENTATION('density',(#14033),#27018);
#14265=REPRESENTATION('material name',(#14379),#27019);
#14266=REPRESENTATION('density',(#14034),#27019);
#14267=REPRESENTATION('material name',(#14380),#27020);
#14268=REPRESENTATION('density',(#14035),#27020);
#14269=REPRESENTATION('material name',(#14381),#27021);
#14270=REPRESENTATION('density',(#14036),#27021);
#14271=REPRESENTATION('material name',(#14382),#27023);
#14272=REPRESENTATION('density',(#14037),#27023);
#14273=REPRESENTATION('material name',(#14383),#27024);
#14274=REPRESENTATION('density',(#14038),#27024);
#14275=REPRESENTATION('material name',(#14384),#27025);
#14276=REPRESENTATION('density',(#14039),#27025);
#14277=REPRESENTATION('material name',(#14385),#27026);
#14278=REPRESENTATION('density',(#14040),#27026);
#14279=REPRESENTATION('material name',(#14386),#27027);
#14280=REPRESENTATION('density',(#14041),#27027);
#14281=REPRESENTATION('material name',(#14387),#27028);
#14282=REPRESENTATION('density',(#14042),#27028);
#14283=REPRESENTATION('material name',(#14388),#27030);
#14284=REPRESENTATION('density',(#14043),#27030);
#14285=REPRESENTATION('material name',(#14389),#27031);
#14286=REPRESENTATION('density',(#14044),#27031);
#14287=REPRESENTATION('material name',(#14390),#27032);
#14288=REPRESENTATION('density',(#14045),#27032);
#14289=REPRESENTATION('material name',(#14391),#27033);
#14290=REPRESENTATION('density',(#14046),#27033);
#14291=REPRESENTATION('material name',(#14392),#27034);
#14292=REPRESENTATION('density',(#14047),#27034);
#14293=REPRESENTATION('material name',(#14393),#27035);
#14294=REPRESENTATION('density',(#14048),#27035);
#14295=REPRESENTATION('material name',(#14394),#27037);
#14296=REPRESENTATION('density',(#14049),#27037);
#14297=REPRESENTATION('material name',(#14395),#27038);
#14298=REPRESENTATION('density',(#14050),#27038);
#14299=REPRESENTATION('material name',(#14396),#27039);
#14300=REPRESENTATION('density',(#14051),#27039);
#14301=REPRESENTATION('material name',(#14397),#27040);
#14302=REPRESENTATION('density',(#14052),#27040);
#14303=REPRESENTATION('material name',(#14398),#27041);
#14304=REPRESENTATION('density',(#14053),#27041);
#14305=REPRESENTATION('material name',(#14399),#27043);
#14306=REPRESENTATION('density',(#14054),#27043);
#14307=REPRESENTATION('material name',(#14400),#27044);
#14308=REPRESENTATION('density',(#14055),#27044);
#14309=REPRESENTATION('material name',(#14401),#27045);
#14310=REPRESENTATION('density',(#14056),#27045);
#14311=REPRESENTATION('material name',(#14402),#27046);
#14312=REPRESENTATION('density',(#14057),#27046);
#14313=REPRESENTATION('material name',(#14403),#27047);
#14314=REPRESENTATION('density',(#14058),#27047);
#14315=REPRESENTATION('material name',(#14404),#27048);
#14316=REPRESENTATION('density',(#14059),#27048);
#14317=REPRESENTATION('material name',(#14405),#27049);
#14318=REPRESENTATION('density',(#14060),#27049);
#14319=REPRESENTATION('material name',(#14406),#27050);
#14320=REPRESENTATION('density',(#14061),#27050);
#14321=REPRESENTATION('material name',(#14407),#27051);
#14322=REPRESENTATION('density',(#14062),#27051);
#14323=REPRESENTATION('material name',(#14408),#27053);
#14324=REPRESENTATION('density',(#14063),#27053);
#14325=REPRESENTATION('material name',(#14409),#27054);
#14326=REPRESENTATION('density',(#14064),#27054);
#14327=REPRESENTATION('material name',(#14410),#27055);
#14328=REPRESENTATION('density',(#14065),#27055);
#14329=REPRESENTATION('material name',(#14411),#27056);
#14330=REPRESENTATION('density',(#14066),#27056);
#14331=REPRESENTATION('material name',(#14412),#27057);
#14332=REPRESENTATION('density',(#14067),#27057);
#14333=REPRESENTATION('material name',(#14413),#27058);
#14334=REPRESENTATION('density',(#14068),#27058);
#14335=REPRESENTATION('material name',(#14414),#27059);
#14336=REPRESENTATION('density',(#14069),#27059);
#14337=REPRESENTATION('material name',(#14415),#27060);
#14338=REPRESENTATION('density',(#14070),#27060);
#14339=REPRESENTATION('material name',(#14416),#27061);
#14340=REPRESENTATION('density',(#14071),#27061);
#14341=REPRESENTATION('material name',(#14417),#27062);
#14342=REPRESENTATION('density',(#14072),#27062);
#14343=REPRESENTATION('material name',(#14418),#27063);
#14344=REPRESENTATION('density',(#14073),#27063);
#14345=REPRESENTATION('material name',(#14419),#27064);
#14346=REPRESENTATION('density',(#14074),#27064);
#14347=REPRESENTATION('material name',(#14420),#27065);
#14348=REPRESENTATION('density',(#14075),#27065);
#14349=REPRESENTATION('material name',(#14421),#27066);
#14350=REPRESENTATION('density',(#14076),#27066);
#14351=REPRESENTATION('material name',(#14422),#27067);
#14352=REPRESENTATION('density',(#14077),#27067);
#14353=REPRESENTATION('material name',(#14423),#27068);
#14354=REPRESENTATION('density',(#14078),#27068);
#14355=DESCRIPTIVE_REPRESENTATION_ITEM('Steel','Steel');
#14356=DESCRIPTIVE_REPRESENTATION_ITEM('Steel','Steel');
#14357=DESCRIPTIVE_REPRESENTATION_ITEM('Steel','Steel');
#14358=DESCRIPTIVE_REPRESENTATION_ITEM('Steel','Steel');
#14359=DESCRIPTIVE_REPRESENTATION_ITEM('Steel','Steel');
#14360=DESCRIPTIVE_REPRESENTATION_ITEM('Steel','Steel');
#14361=DESCRIPTIVE_REPRESENTATION_ITEM('Steel','Steel');
#14362=DESCRIPTIVE_REPRESENTATION_ITEM('Steel','Steel');
#14363=DESCRIPTIVE_REPRESENTATION_ITEM('Steel','Steel');
#14364=DESCRIPTIVE_REPRESENTATION_ITEM('Steel','Steel');
#14365=DESCRIPTIVE_REPRESENTATION_ITEM('Steel','Steel');
#14366=DESCRIPTIVE_REPRESENTATION_ITEM('Steel','Steel');
#14367=DESCRIPTIVE_REPRESENTATION_ITEM('Steel','Steel');
#14368=DESCRIPTIVE_REPRESENTATION_ITEM('Steel','Steel');
#14369=DESCRIPTIVE_REPRESENTATION_ITEM('Steel','Steel');
#14370=DESCRIPTIVE_REPRESENTATION_ITEM('Steel','Steel');
#14371=DESCRIPTIVE_REPRESENTATION_ITEM('Steel','Steel');
#14372=DESCRIPTIVE_REPRESENTATION_ITEM('Steel','Steel');
#14373=DESCRIPTIVE_REPRESENTATION_ITEM('Steel','Steel');
#14374=DESCRIPTIVE_REPRESENTATION_ITEM('Steel','Steel');
#14375=DESCRIPTIVE_REPRESENTATION_ITEM('Steel','Steel');
#14376=DESCRIPTIVE_REPRESENTATION_ITEM('Steel','Steel');
#14377=DESCRIPTIVE_REPRESENTATION_ITEM('Steel','Steel');
#14378=DESCRIPTIVE_REPRESENTATION_ITEM('Steel','Steel');
#14379=DESCRIPTIVE_REPRESENTATION_ITEM('Steel','Steel');
#14380=DESCRIPTIVE_REPRESENTATION_ITEM('Steel','Steel');
#14381=DESCRIPTIVE_REPRESENTATION_ITEM('Steel','Steel');
#14382=DESCRIPTIVE_REPRESENTATION_ITEM('Steel','Steel');
#14383=DESCRIPTIVE_REPRESENTATION_ITEM('Steel','Steel');
#14384=DESCRIPTIVE_REPRESENTATION_ITEM('Steel','Steel');
#14385=DESCRIPTIVE_REPRESENTATION_ITEM('Steel','Steel');
#14386=DESCRIPTIVE_REPRESENTATION_ITEM('Steel','Steel');
#14387=DESCRIPTIVE_REPRESENTATION_ITEM('Steel','Steel');
#14388=DESCRIPTIVE_REPRESENTATION_ITEM('Steel','Steel');
#14389=DESCRIPTIVE_REPRESENTATION_ITEM('Steel','Steel');
#14390=DESCRIPTIVE_REPRESENTATION_ITEM('Steel','Steel');
#14391=DESCRIPTIVE_REPRESENTATION_ITEM('Steel','Steel');
#14392=DESCRIPTIVE_REPRESENTATION_ITEM('Steel','Steel');
#14393=DESCRIPTIVE_REPRESENTATION_ITEM('Steel','Steel');
#14394=DESCRIPTIVE_REPRESENTATION_ITEM('Steel','Steel');
#14395=DESCRIPTIVE_REPRESENTATION_ITEM('Steel','Steel');
#14396=DESCRIPTIVE_REPRESENTATION_ITEM('Steel','Steel');
#14397=DESCRIPTIVE_REPRESENTATION_ITEM('Steel','Steel');
#14398=DESCRIPTIVE_REPRESENTATION_ITEM('Steel','Steel');
#14399=DESCRIPTIVE_REPRESENTATION_ITEM('Steel','Steel');
#14400=DESCRIPTIVE_REPRESENTATION_ITEM('Steel','Steel');
#14401=DESCRIPTIVE_REPRESENTATION_ITEM('Steel','Steel');
#14402=DESCRIPTIVE_REPRESENTATION_ITEM('Steel','Steel');
#14403=DESCRIPTIVE_REPRESENTATION_ITEM('Steel','Steel');
#14404=DESCRIPTIVE_REPRESENTATION_ITEM('Steel','Steel');
#14405=DESCRIPTIVE_REPRESENTATION_ITEM('Steel','Steel');
#14406=DESCRIPTIVE_REPRESENTATION_ITEM('Steel','Steel');
#14407=DESCRIPTIVE_REPRESENTATION_ITEM('Steel','Steel');
#14408=DESCRIPTIVE_REPRESENTATION_ITEM('Steel','Steel');
#14409=DESCRIPTIVE_REPRESENTATION_ITEM('Steel','Steel');
#14410=DESCRIPTIVE_REPRESENTATION_ITEM('Steel','Steel');
#14411=DESCRIPTIVE_REPRESENTATION_ITEM('Steel','Steel');
#14412=DESCRIPTIVE_REPRESENTATION_ITEM('Steel','Steel');
#14413=DESCRIPTIVE_REPRESENTATION_ITEM('Steel','Steel');
#14414=DESCRIPTIVE_REPRESENTATION_ITEM('Steel','Steel');
#14415=DESCRIPTIVE_REPRESENTATION_ITEM('Steel','Steel');
#14416=DESCRIPTIVE_REPRESENTATION_ITEM('Steel','Steel');
#14417=DESCRIPTIVE_REPRESENTATION_ITEM('Steel','Steel');
#14418=DESCRIPTIVE_REPRESENTATION_ITEM('Steel','Steel');
#14419=DESCRIPTIVE_REPRESENTATION_ITEM('Steel','Steel');
#14420=DESCRIPTIVE_REPRESENTATION_ITEM('Steel','Steel');
#14421=DESCRIPTIVE_REPRESENTATION_ITEM('Steel','Steel');
#14422=DESCRIPTIVE_REPRESENTATION_ITEM('Steel','Steel');
#14423=DESCRIPTIVE_REPRESENTATION_ITEM('Steel','Steel');
#14424=PROPERTY_DEFINITION('material property','material name',#27430);
#14425=PROPERTY_DEFINITION('material property','density of part',#27430);
#14426=PROPERTY_DEFINITION('material property','material name',#27431);
#14427=PROPERTY_DEFINITION('material property','density of part',#27431);
#14428=PROPERTY_DEFINITION('material property','material name',#27432);
#14429=PROPERTY_DEFINITION('material property','density of part',#27432);
#14430=PROPERTY_DEFINITION('material property','material name',#27433);
#14431=PROPERTY_DEFINITION('material property','density of part',#27433);
#14432=PROPERTY_DEFINITION('material property','material name',#27434);
#14433=PROPERTY_DEFINITION('material property','density of part',#27434);
#14434=PROPERTY_DEFINITION('material property','material name',#27435);
#14435=PROPERTY_DEFINITION('material property','density of part',#27435);
#14436=PROPERTY_DEFINITION('material property','material name',#27436);
#14437=PROPERTY_DEFINITION('material property','density of part',#27436);
#14438=PROPERTY_DEFINITION('material property','material name',#27437);
#14439=PROPERTY_DEFINITION('material property','density of part',#27437);
#14440=PROPERTY_DEFINITION('material property','material name',#27438);
#14441=PROPERTY_DEFINITION('material property','density of part',#27438);
#14442=PROPERTY_DEFINITION('material property','material name',#27439);
#14443=PROPERTY_DEFINITION('material property','density of part',#27439);
#14444=PROPERTY_DEFINITION('material property','material name',#27440);
#14445=PROPERTY_DEFINITION('material property','density of part',#27440);
#14446=PROPERTY_DEFINITION('material property','material name',#27441);
#14447=PROPERTY_DEFINITION('material property','density of part',#27441);
#14448=PROPERTY_DEFINITION('material property','material name',#27442);
#14449=PROPERTY_DEFINITION('material property','density of part',#27442);
#14450=PROPERTY_DEFINITION('material property','material name',#27443);
#14451=PROPERTY_DEFINITION('material property','density of part',#27443);
#14452=PROPERTY_DEFINITION('material property','material name',#27444);
#14453=PROPERTY_DEFINITION('material property','density of part',#27444);
#14454=PROPERTY_DEFINITION('material property','material name',#27445);
#14455=PROPERTY_DEFINITION('material property','density of part',#27445);
#14456=PROPERTY_DEFINITION('material property','material name',#27446);
#14457=PROPERTY_DEFINITION('material property','density of part',#27446);
#14458=PROPERTY_DEFINITION('material property','material name',#27447);
#14459=PROPERTY_DEFINITION('material property','density of part',#27447);
#14460=PROPERTY_DEFINITION('material property','material name',#27448);
#14461=PROPERTY_DEFINITION('material property','density of part',#27448);
#14462=PROPERTY_DEFINITION('material property','material name',#27449);
#14463=PROPERTY_DEFINITION('material property','density of part',#27449);
#14464=PROPERTY_DEFINITION('material property','material name',#27450);
#14465=PROPERTY_DEFINITION('material property','density of part',#27450);
#14466=PROPERTY_DEFINITION('material property','material name',#27451);
#14467=PROPERTY_DEFINITION('material property','density of part',#27451);
#14468=PROPERTY_DEFINITION('material property','material name',#27452);
#14469=PROPERTY_DEFINITION('material property','density of part',#27452);
#14470=PROPERTY_DEFINITION('material property','material name',#27453);
#14471=PROPERTY_DEFINITION('material property','density of part',#27453);
#14472=PROPERTY_DEFINITION('material property','material name',#27454);
#14473=PROPERTY_DEFINITION('material property','density of part',#27454);
#14474=PROPERTY_DEFINITION('material property','material name',#27455);
#14475=PROPERTY_DEFINITION('material property','density of part',#27455);
#14476=PROPERTY_DEFINITION('material property','material name',#27456);
#14477=PROPERTY_DEFINITION('material property','density of part',#27456);
#14478=PROPERTY_DEFINITION('material property','material name',#27458);
#14479=PROPERTY_DEFINITION('material property','density of part',#27458);
#14480=PROPERTY_DEFINITION('material property','material name',#27459);
#14481=PROPERTY_DEFINITION('material property','density of part',#27459);
#14482=PROPERTY_DEFINITION('material property','material name',#27460);
#14483=PROPERTY_DEFINITION('material property','density of part',#27460);
#14484=PROPERTY_DEFINITION('material property','material name',#27461);
#14485=PROPERTY_DEFINITION('material property','density of part',#27461);
#14486=PROPERTY_DEFINITION('material property','material name',#27462);
#14487=PROPERTY_DEFINITION('material property','density of part',#27462);
#14488=PROPERTY_DEFINITION('material property','material name',#27463);
#14489=PROPERTY_DEFINITION('material property','density of part',#27463);
#14490=PROPERTY_DEFINITION('material property','material name',#27465);
#14491=PROPERTY_DEFINITION('material property','density of part',#27465);
#14492=PROPERTY_DEFINITION('material property','material name',#27466);
#14493=PROPERTY_DEFINITION('material property','density of part',#27466);
#14494=PROPERTY_DEFINITION('material property','material name',#27467);
#14495=PROPERTY_DEFINITION('material property','density of part',#27467);
#14496=PROPERTY_DEFINITION('material property','material name',#27468);
#14497=PROPERTY_DEFINITION('material property','density of part',#27468);
#14498=PROPERTY_DEFINITION('material property','material name',#27469);
#14499=PROPERTY_DEFINITION('material property','density of part',#27469);
#14500=PROPERTY_DEFINITION('material property','material name',#27470);
#14501=PROPERTY_DEFINITION('material property','density of part',#27470);
#14502=PROPERTY_DEFINITION('material property','material name',#27472);
#14503=PROPERTY_DEFINITION('material property','density of part',#27472);
#14504=PROPERTY_DEFINITION('material property','material name',#27473);
#14505=PROPERTY_DEFINITION('material property','density of part',#27473);
#14506=PROPERTY_DEFINITION('material property','material name',#27474);
#14507=PROPERTY_DEFINITION('material property','density of part',#27474);
#14508=PROPERTY_DEFINITION('material property','material name',#27475);
#14509=PROPERTY_DEFINITION('material property','density of part',#27475);
#14510=PROPERTY_DEFINITION('material property','material name',#27476);
#14511=PROPERTY_DEFINITION('material property','density of part',#27476);
#14512=PROPERTY_DEFINITION('material property','material name',#27478);
#14513=PROPERTY_DEFINITION('material property','density of part',#27478);
#14514=PROPERTY_DEFINITION('material property','material name',#27479);
#14515=PROPERTY_DEFINITION('material property','density of part',#27479);
#14516=PROPERTY_DEFINITION('material property','material name',#27480);
#14517=PROPERTY_DEFINITION('material property','density of part',#27480);
#14518=PROPERTY_DEFINITION('material property','material name',#27481);
#14519=PROPERTY_DEFINITION('material property','density of part',#27481);
#14520=PROPERTY_DEFINITION('material property','material name',#27482);
#14521=PROPERTY_DEFINITION('material property','density of part',#27482);
#14522=PROPERTY_DEFINITION('material property','material name',#27483);
#14523=PROPERTY_DEFINITION('material property','density of part',#27483);
#14524=PROPERTY_DEFINITION('material property','material name',#27484);
#14525=PROPERTY_DEFINITION('material property','density of part',#27484);
#14526=PROPERTY_DEFINITION('material property','material name',#27485);
#14527=PROPERTY_DEFINITION('material property','density of part',#27485);
#14528=PROPERTY_DEFINITION('material property','material name',#27486);
#14529=PROPERTY_DEFINITION('material property','density of part',#27486);
#14530=PROPERTY_DEFINITION('material property','material name',#27488);
#14531=PROPERTY_DEFINITION('material property','density of part',#27488);
#14532=PROPERTY_DEFINITION('material property','material name',#27489);
#14533=PROPERTY_DEFINITION('material property','density of part',#27489);
#14534=PROPERTY_DEFINITION('material property','material name',#27490);
#14535=PROPERTY_DEFINITION('material property','density of part',#27490);
#14536=PROPERTY_DEFINITION('material property','material name',#27491);
#14537=PROPERTY_DEFINITION('material property','density of part',#27491);
#14538=PROPERTY_DEFINITION('material property','material name',#27492);
#14539=PROPERTY_DEFINITION('material property','density of part',#27492);
#14540=PROPERTY_DEFINITION('material property','material name',#27493);
#14541=PROPERTY_DEFINITION('material property','density of part',#27493);
#14542=PROPERTY_DEFINITION('material property','material name',#27494);
#14543=PROPERTY_DEFINITION('material property','density of part',#27494);
#14544=PROPERTY_DEFINITION('material property','material name',#27495);
#14545=PROPERTY_DEFINITION('material property','density of part',#27495);
#14546=PROPERTY_DEFINITION('material property','material name',#27496);
#14547=PROPERTY_DEFINITION('material property','density of part',#27496);
#14548=PROPERTY_DEFINITION('material property','material name',#27497);
#14549=PROPERTY_DEFINITION('material property','density of part',#27497);
#14550=PROPERTY_DEFINITION('material property','material name',#27498);
#14551=PROPERTY_DEFINITION('material property','density of part',#27498);
#14552=PROPERTY_DEFINITION('material property','material name',#27499);
#14553=PROPERTY_DEFINITION('material property','density of part',#27499);
#14554=PROPERTY_DEFINITION('material property','material name',#27500);
#14555=PROPERTY_DEFINITION('material property','density of part',#27500);
#14556=PROPERTY_DEFINITION('material property','material name',#27501);
#14557=PROPERTY_DEFINITION('material property','density of part',#27501);
#14558=PROPERTY_DEFINITION('material property','material name',#27502);
#14559=PROPERTY_DEFINITION('material property','density of part',#27502);
#14560=PROPERTY_DEFINITION('material property','material name',#27503);
#14561=PROPERTY_DEFINITION('material property','density of part',#27503);
#14562=AXIS2_PLACEMENT_3D('',#20970,#16434,#16435);
#14563=AXIS2_PLACEMENT_3D('',#20971,#16436,#16437);
#14564=AXIS2_PLACEMENT_3D('',#20972,#16438,#16439);
#14565=AXIS2_PLACEMENT_3D('',#20973,#16440,#16441);
#14566=AXIS2_PLACEMENT_3D('',#20975,#16442,#16443);
#14567=AXIS2_PLACEMENT_3D('',#20978,#16445,#16446);
#14568=AXIS2_PLACEMENT_3D('',#20979,#16447,#16448);
#14569=AXIS2_PLACEMENT_3D('',#20980,#16449,#16450);
#14570=AXIS2_PLACEMENT_3D('',#20982,#16451,#16452);
#14571=AXIS2_PLACEMENT_3D('',#20985,#16454,#16455);
#14572=AXIS2_PLACEMENT_3D('',#20986,#16456,#16457);
#14573=AXIS2_PLACEMENT_3D('',#20987,#16458,#16459);
#14574=AXIS2_PLACEMENT_3D('',#20989,#16460,#16461);
#14575=AXIS2_PLACEMENT_3D('',#20992,#16463,#16464);
#14576=AXIS2_PLACEMENT_3D('',#20993,#16465,#16466);
#14577=AXIS2_PLACEMENT_3D('',#20994,#16467,#16468);
#14578=AXIS2_PLACEMENT_3D('',#20996,#16469,#16470);
#14579=AXIS2_PLACEMENT_3D('',#20999,#16472,#16473);
#14580=AXIS2_PLACEMENT_3D('',#21000,#16474,#16475);
#14581=AXIS2_PLACEMENT_3D('',#21001,#16476,#16477);
#14582=AXIS2_PLACEMENT_3D('',#21003,#16478,#16479);
#14583=AXIS2_PLACEMENT_3D('',#21006,#16481,#16482);
#14584=AXIS2_PLACEMENT_3D('',#21007,#16483,#16484);
#14585=AXIS2_PLACEMENT_3D('',#21008,#16485,#16486);
#14586=AXIS2_PLACEMENT_3D('',#21010,#16487,#16488);
#14587=AXIS2_PLACEMENT_3D('',#21013,#16490,#16491);
#14588=AXIS2_PLACEMENT_3D('',#21014,#16492,#16493);
#14589=AXIS2_PLACEMENT_3D('',#21015,#16494,#16495);
#14590=AXIS2_PLACEMENT_3D('',#21017,#16496,#16497);
#14591=AXIS2_PLACEMENT_3D('',#21020,#16499,#16500);
#14592=AXIS2_PLACEMENT_3D('',#21021,#16501,#16502);
#14593=AXIS2_PLACEMENT_3D('',#21022,#16503,#16504);
#14594=AXIS2_PLACEMENT_3D('',#21024,#16505,#16506);
#14595=AXIS2_PLACEMENT_3D('',#21027,#16508,#16509);
#14596=AXIS2_PLACEMENT_3D('',#21028,#16510,#16511);
#14597=AXIS2_PLACEMENT_3D('',#21029,#16512,#16513);
#14598=AXIS2_PLACEMENT_3D('',#21031,#16514,#16515);
#14599=AXIS2_PLACEMENT_3D('',#21034,#16517,#16518);
#14600=AXIS2_PLACEMENT_3D('',#21035,#16519,#16520);
#14601=AXIS2_PLACEMENT_3D('',#21036,#16521,#16522);
#14602=AXIS2_PLACEMENT_3D('',#21038,#16523,#16524);
#14603=AXIS2_PLACEMENT_3D('',#21041,#16526,#16527);
#14604=AXIS2_PLACEMENT_3D('',#21042,#16528,#16529);
#14605=AXIS2_PLACEMENT_3D('',#21043,#16530,#16531);
#14606=AXIS2_PLACEMENT_3D('',#21048,#16533,#16534);
#14607=AXIS2_PLACEMENT_3D('',#21051,#16536,#16537);
#14608=AXIS2_PLACEMENT_3D('',#21052,#16538,#16539);
#14609=AXIS2_PLACEMENT_3D('',#21057,#16541,#16542);
#14610=AXIS2_PLACEMENT_3D('',#21060,#16544,#16545);
#14611=AXIS2_PLACEMENT_3D('',#21061,#16546,#16547);
#14612=AXIS2_PLACEMENT_3D('',#21072,#16552,#16553);
#14613=AXIS2_PLACEMENT_3D('',#21076,#16555,#16556);
#14614=AXIS2_PLACEMENT_3D('',#21080,#16558,#16559);
#14615=AXIS2_PLACEMENT_3D('',#21084,#16561,#16562);
#14616=AXIS2_PLACEMENT_3D('',#21088,#16564,#16565);
#14617=AXIS2_PLACEMENT_3D('',#21092,#16567,#16568);
#14618=AXIS2_PLACEMENT_3D('',#21096,#16572,#16573);
#14619=AXIS2_PLACEMENT_3D('',#21098,#16575,#16576);
#14620=AXIS2_PLACEMENT_3D('',#21100,#16578,#16579);
#14621=AXIS2_PLACEMENT_3D('',#21105,#16582,#16583);
#14622=AXIS2_PLACEMENT_3D('',#21106,#16584,#16585);
#14623=AXIS2_PLACEMENT_3D('',#21110,#16587,#16588);
#14624=AXIS2_PLACEMENT_3D('',#21112,#16590,#16591);
#14625=AXIS2_PLACEMENT_3D('',#21114,#16593,#16594);
#14626=AXIS2_PLACEMENT_3D('',#21116,#16596,#16597);
#14627=AXIS2_PLACEMENT_3D('',#21121,#16599,#16600);
#14628=AXIS2_PLACEMENT_3D('',#21126,#16603,#16604);
#14629=AXIS2_PLACEMENT_3D('',#21129,#16606,#16607);
#14630=AXIS2_PLACEMENT_3D('',#21130,#16608,#16609);
#14631=AXIS2_PLACEMENT_3D('',#21134,#16611,#16612);
#14632=AXIS2_PLACEMENT_3D('',#21136,#16614,#16615);
#14633=AXIS2_PLACEMENT_3D('',#21138,#16617,#16618);
#14634=AXIS2_PLACEMENT_3D('',#21140,#16620,#16621);
#14635=AXIS2_PLACEMENT_3D('',#21145,#16623,#16624);
#14636=AXIS2_PLACEMENT_3D('',#21150,#16627,#16628);
#14637=AXIS2_PLACEMENT_3D('',#21153,#16630,#16631);
#14638=AXIS2_PLACEMENT_3D('',#21154,#16632,#16633);
#14639=AXIS2_PLACEMENT_3D('',#21158,#16635,#16636);
#14640=AXIS2_PLACEMENT_3D('',#21160,#16638,#16639);
#14641=AXIS2_PLACEMENT_3D('',#21162,#16641,#16642);
#14642=AXIS2_PLACEMENT_3D('',#21164,#16644,#16645);
#14643=AXIS2_PLACEMENT_3D('',#21165,#16646,#16647);
#14644=AXIS2_PLACEMENT_3D('',#21166,#16648,#16649);
#14645=AXIS2_PLACEMENT_3D('',#21167,#16650,#16651);
#14646=AXIS2_PLACEMENT_3D('',#21168,#16652,#16653);
#14647=AXIS2_PLACEMENT_3D('',#21170,#16654,#16655);
#14648=AXIS2_PLACEMENT_3D('',#21173,#16657,#16658);
#14649=AXIS2_PLACEMENT_3D('',#21174,#16659,#16660);
#14650=AXIS2_PLACEMENT_3D('',#21175,#16661,#16662);
#14651=AXIS2_PLACEMENT_3D('',#21177,#16663,#16664);
#14652=AXIS2_PLACEMENT_3D('',#21180,#16666,#16667);
#14653=AXIS2_PLACEMENT_3D('',#21181,#16668,#16669);
#14654=AXIS2_PLACEMENT_3D('',#21182,#16670,#16671);
#14655=AXIS2_PLACEMENT_3D('',#21183,#16672,#16673);
#14656=AXIS2_PLACEMENT_3D('',#21184,#16674,#16675);
#14657=AXIS2_PLACEMENT_3D('',#21185,#16676,#16677);
#14658=AXIS2_PLACEMENT_3D('',#21186,#16678,#16679);
#14659=AXIS2_PLACEMENT_3D('',#21192,#16683,#16684);
#14660=AXIS2_PLACEMENT_3D('',#21196,#16687,#16688);
#14661=AXIS2_PLACEMENT_3D('',#21200,#16691,#16692);
#14662=AXIS2_PLACEMENT_3D('',#21202,#16694,#16695);
#14663=AXIS2_PLACEMENT_3D('',#21203,#16696,#16697);
#14664=AXIS2_PLACEMENT_3D('',#21204,#16698,#16699);
#14665=AXIS2_PLACEMENT_3D('',#21213,#16704,#16705);
#14666=AXIS2_PLACEMENT_3D('',#21219,#16709,#16710);
#14667=AXIS2_PLACEMENT_3D('',#21225,#16714,#16715);
#14668=AXIS2_PLACEMENT_3D('',#21228,#16718,#16719);
#14669=AXIS2_PLACEMENT_3D('',#21229,#16720,#16721);
#14670=AXIS2_PLACEMENT_3D('',#21230,#16722,#16723);
#14671=AXIS2_PLACEMENT_3D('',#21231,#16724,#16725);
#14672=AXIS2_PLACEMENT_3D('',#21240,#16730,#16731);
#14673=AXIS2_PLACEMENT_3D('',#21246,#16735,#16736);
#14674=AXIS2_PLACEMENT_3D('',#21252,#16740,#16741);
#14675=AXIS2_PLACEMENT_3D('',#21255,#16744,#16745);
#14676=AXIS2_PLACEMENT_3D('',#21256,#16746,#16747);
#14677=AXIS2_PLACEMENT_3D('',#21257,#16748,#16749);
#14678=AXIS2_PLACEMENT_3D('',#21258,#16750,#16751);
#14679=AXIS2_PLACEMENT_3D('',#21260,#16752,#16753);
#14680=AXIS2_PLACEMENT_3D('',#21263,#16755,#16756);
#14681=AXIS2_PLACEMENT_3D('',#21264,#16757,#16758);
#14682=AXIS2_PLACEMENT_3D('',#21266,#16759,#16760);
#14683=AXIS2_PLACEMENT_3D('',#21269,#16762,#16763);
#14684=AXIS2_PLACEMENT_3D('',#21270,#16764,#16765);
#14685=AXIS2_PLACEMENT_3D('',#21272,#16766,#16767);
#14686=AXIS2_PLACEMENT_3D('',#21275,#16769,#16770);
#14687=AXIS2_PLACEMENT_3D('',#21276,#16771,#16772);
#14688=AXIS2_PLACEMENT_3D('',#21278,#16773,#16774);
#14689=AXIS2_PLACEMENT_3D('',#21281,#16776,#16777);
#14690=AXIS2_PLACEMENT_3D('',#21282,#16778,#16779);
#14691=AXIS2_PLACEMENT_3D('',#21284,#16780,#16781);
#14692=AXIS2_PLACEMENT_3D('',#21287,#16783,#16784);
#14693=AXIS2_PLACEMENT_3D('',#21288,#16785,#16786);
#14694=AXIS2_PLACEMENT_3D('',#21290,#16787,#16788);
#14695=AXIS2_PLACEMENT_3D('',#21293,#16790,#16791);
#14696=AXIS2_PLACEMENT_3D('',#21294,#16792,#16793);
#14697=AXIS2_PLACEMENT_3D('',#21296,#16794,#16795);
#14698=AXIS2_PLACEMENT_3D('',#21299,#16797,#16798);
#14699=AXIS2_PLACEMENT_3D('',#21300,#16799,#16800);
#14700=AXIS2_PLACEMENT_3D('',#21302,#16801,#16802);
#14701=AXIS2_PLACEMENT_3D('',#21305,#16804,#16805);
#14702=AXIS2_PLACEMENT_3D('',#21306,#16806,#16807);
#14703=AXIS2_PLACEMENT_3D('',#21308,#16808,#16809);
#14704=AXIS2_PLACEMENT_3D('',#21311,#16811,#16812);
#14705=AXIS2_PLACEMENT_3D('',#21312,#16813,#16814);
#14706=AXIS2_PLACEMENT_3D('',#21321,#16819,#16820);
#14707=AXIS2_PLACEMENT_3D('',#21330,#16825,#16826);
#14708=AXIS2_PLACEMENT_3D('',#21336,#16830,#16831);
#14709=AXIS2_PLACEMENT_3D('',#21342,#16835,#16836);
#14710=AXIS2_PLACEMENT_3D('',#21349,#16841,#16842);
#14711=AXIS2_PLACEMENT_3D('',#21353,#16845,#16846);
#14712=AXIS2_PLACEMENT_3D('',#21358,#16850,#16851);
#14713=AXIS2_PLACEMENT_3D('',#21360,#16853,#16854);
#14714=AXIS2_PLACEMENT_3D('',#21361,#16855,#16856);
#14715=AXIS2_PLACEMENT_3D('',#21362,#16857,#16858);
#14716=AXIS2_PLACEMENT_3D('',#21363,#16859,#16860);
#14717=AXIS2_PLACEMENT_3D('',#21365,#16861,#16862);
#14718=AXIS2_PLACEMENT_3D('',#21368,#16864,#16865);
#14719=AXIS2_PLACEMENT_3D('',#21369,#16866,#16867);
#14720=AXIS2_PLACEMENT_3D('',#21371,#16868,#16869);
#14721=AXIS2_PLACEMENT_3D('',#21374,#16871,#16872);
#14722=AXIS2_PLACEMENT_3D('',#21375,#16873,#16874);
#14723=AXIS2_PLACEMENT_3D('',#21376,#16875,#16876);
#14724=AXIS2_PLACEMENT_3D('',#21377,#16877,#16878);
#14725=AXIS2_PLACEMENT_3D('',#21378,#16879,#16880);
#14726=AXIS2_PLACEMENT_3D('',#21383,#16882,#16883);
#14727=AXIS2_PLACEMENT_3D('',#21386,#16885,#16886);
#14728=AXIS2_PLACEMENT_3D('',#21387,#16887,#16888);
#14729=AXIS2_PLACEMENT_3D('',#21392,#16890,#16891);
#14730=AXIS2_PLACEMENT_3D('',#21395,#16893,#16894);
#14731=AXIS2_PLACEMENT_3D('',#21396,#16895,#16896);
#14732=AXIS2_PLACEMENT_3D('',#21401,#16898,#16899);
#14733=AXIS2_PLACEMENT_3D('',#21404,#16901,#16902);
#14734=AXIS2_PLACEMENT_3D('',#21405,#16903,#16904);
#14735=AXIS2_PLACEMENT_3D('',#21410,#16906,#16907);
#14736=AXIS2_PLACEMENT_3D('',#21413,#16909,#16910);
#14737=AXIS2_PLACEMENT_3D('',#21414,#16911,#16912);
#14738=AXIS2_PLACEMENT_3D('',#21415,#16913,#16914);
#14739=AXIS2_PLACEMENT_3D('',#21416,#16915,#16916);
#14740=AXIS2_PLACEMENT_3D('',#21417,#16917,#16918);
#14741=AXIS2_PLACEMENT_3D('',#21418,#16919,#16920);
#14742=AXIS2_PLACEMENT_3D('',#21420,#16921,#16922);
#14743=AXIS2_PLACEMENT_3D('',#21421,#16923,#16924);
#14744=AXIS2_PLACEMENT_3D('',#21422,#16925,#16926);
#14745=AXIS2_PLACEMENT_3D('',#21423,#16927,#16928);
#14746=AXIS2_PLACEMENT_3D('',#21424,#16929,#16930);
#14747=AXIS2_PLACEMENT_3D('',#21425,#16931,#16932);
#14748=AXIS2_PLACEMENT_3D('',#21426,#16933,#16934);
#14749=AXIS2_PLACEMENT_3D('',#21427,#16935,#16936);
#14750=AXIS2_PLACEMENT_3D('',#21428,#16937,#16938);
#14751=AXIS2_PLACEMENT_3D('',#21429,#16939,#16940);
#14752=AXIS2_PLACEMENT_3D('',#21431,#16941,#16942);
#14753=AXIS2_PLACEMENT_3D('',#21434,#16944,#16945);
#14754=AXIS2_PLACEMENT_3D('',#21435,#16946,#16947);
#14755=AXIS2_PLACEMENT_3D('',#21437,#16948,#16949);
#14756=AXIS2_PLACEMENT_3D('',#21438,#16950,#16951);
#14757=AXIS2_PLACEMENT_3D('',#21440,#16953,#16954);
#14758=AXIS2_PLACEMENT_3D('',#21441,#16955,#16956);
#14759=AXIS2_PLACEMENT_3D('',#21442,#16957,#16958);
#14760=AXIS2_PLACEMENT_3D('',#21447,#16960,#16961);
#14761=AXIS2_PLACEMENT_3D('',#21450,#16963,#16964);
#14762=AXIS2_PLACEMENT_3D('',#21451,#16965,#16966);
#14763=AXIS2_PLACEMENT_3D('',#21456,#16968,#16969);
#14764=AXIS2_PLACEMENT_3D('',#21459,#16971,#16972);
#14765=AXIS2_PLACEMENT_3D('',#21460,#16973,#16974);
#14766=AXIS2_PLACEMENT_3D('',#21465,#16976,#16977);
#14767=AXIS2_PLACEMENT_3D('',#21468,#16979,#16980);
#14768=AXIS2_PLACEMENT_3D('',#21469,#16981,#16982);
#14769=AXIS2_PLACEMENT_3D('',#21474,#16984,#16985);
#14770=AXIS2_PLACEMENT_3D('',#21477,#16987,#16988);
#14771=AXIS2_PLACEMENT_3D('',#21478,#16989,#16990);
#14772=AXIS2_PLACEMENT_3D('',#21479,#16991,#16992);
#14773=AXIS2_PLACEMENT_3D('',#21480,#16993,#16994);
#14774=AXIS2_PLACEMENT_3D('',#21481,#16995,#16996);
#14775=AXIS2_PLACEMENT_3D('',#21482,#16997,#16998);
#14776=AXIS2_PLACEMENT_3D('',#21484,#16999,#17000);
#14777=AXIS2_PLACEMENT_3D('',#21485,#17001,#17002);
#14778=AXIS2_PLACEMENT_3D('',#21486,#17003,#17004);
#14779=AXIS2_PLACEMENT_3D('',#21487,#17005,#17006);
#14780=AXIS2_PLACEMENT_3D('',#21488,#17007,#17008);
#14781=AXIS2_PLACEMENT_3D('',#21489,#17009,#17010);
#14782=AXIS2_PLACEMENT_3D('',#21490,#17011,#17012);
#14783=AXIS2_PLACEMENT_3D('',#21491,#17013,#17014);
#14784=AXIS2_PLACEMENT_3D('',#21492,#17015,#17016);
#14785=AXIS2_PLACEMENT_3D('',#21493,#17017,#17018);
#14786=AXIS2_PLACEMENT_3D('',#21496,#17020,#17021);
#14787=AXIS2_PLACEMENT_3D('',#21497,#17022,#17023);
#14788=AXIS2_PLACEMENT_3D('',#21499,#17024,#17025);
#14789=AXIS2_PLACEMENT_3D('',#21500,#17026,#17027);
#14790=AXIS2_PLACEMENT_3D('',#21502,#17028,#17029);
#14791=AXIS2_PLACEMENT_3D('',#21504,#17031,#17032);
#14792=AXIS2_PLACEMENT_3D('',#21505,#17033,#17034);
#14793=AXIS2_PLACEMENT_3D('',#21506,#17035,#17036);
#14794=AXIS2_PLACEMENT_3D('',#21511,#17038,#17039);
#14795=AXIS2_PLACEMENT_3D('',#21514,#17041,#17042);
#14796=AXIS2_PLACEMENT_3D('',#21515,#17043,#17044);
#14797=AXIS2_PLACEMENT_3D('',#21520,#17046,#17047);
#14798=AXIS2_PLACEMENT_3D('',#21523,#17049,#17050);
#14799=AXIS2_PLACEMENT_3D('',#21524,#17051,#17052);
#14800=AXIS2_PLACEMENT_3D('',#21528,#17054,#17055);
#14801=AXIS2_PLACEMENT_3D('',#21532,#17058,#17059);
#14802=AXIS2_PLACEMENT_3D('',#21534,#17060,#17061);
#14803=AXIS2_PLACEMENT_3D('',#21536,#17062,#17063);
#14804=AXIS2_PLACEMENT_3D('',#21538,#17064,#17065);
#14805=AXIS2_PLACEMENT_3D('',#21540,#17066,#17067);
#14806=AXIS2_PLACEMENT_3D('',#21541,#17068,#17069);
#14807=AXIS2_PLACEMENT_3D('',#21545,#17071,#17072);
#14808=AXIS2_PLACEMENT_3D('',#21547,#17074,#17075);
#14809=AXIS2_PLACEMENT_3D('',#21557,#17081,#17082);
#14810=AXIS2_PLACEMENT_3D('',#21564,#17087,#17088);
#14811=AXIS2_PLACEMENT_3D('',#21565,#17089,#17090);
#14812=AXIS2_PLACEMENT_3D('',#21567,#17092,#17093);
#14813=AXIS2_PLACEMENT_3D('',#21569,#17094,#17095);
#14814=AXIS2_PLACEMENT_3D('',#21571,#17097,#17098);
#14815=AXIS2_PLACEMENT_3D('',#21573,#17099,#17100);
#14816=AXIS2_PLACEMENT_3D('',#21575,#17102,#17103);
#14817=AXIS2_PLACEMENT_3D('',#21577,#17104,#17105);
#14818=AXIS2_PLACEMENT_3D('',#21579,#17107,#17108);
#14819=AXIS2_PLACEMENT_3D('',#21581,#17109,#17110);
#14820=AXIS2_PLACEMENT_3D('',#21583,#17112,#17113);
#14821=AXIS2_PLACEMENT_3D('',#21585,#17114,#17115);
#14822=AXIS2_PLACEMENT_3D('',#21587,#17117,#17118);
#14823=AXIS2_PLACEMENT_3D('',#21589,#17119,#17120);
#14824=AXIS2_PLACEMENT_3D('',#21592,#17122,#17123);
#14825=AXIS2_PLACEMENT_3D('',#21593,#17124,#17125);
#14826=AXIS2_PLACEMENT_3D('',#21595,#17126,#17127);
#14827=AXIS2_PLACEMENT_3D('',#21598,#17129,#17130);
#14828=AXIS2_PLACEMENT_3D('',#21599,#17131,#17132);
#14829=AXIS2_PLACEMENT_3D('',#21601,#17133,#17134);
#14830=AXIS2_PLACEMENT_3D('',#21604,#17136,#17137);
#14831=AXIS2_PLACEMENT_3D('',#21605,#17138,#17139);
#14832=AXIS2_PLACEMENT_3D('',#21607,#17140,#17141);
#14833=AXIS2_PLACEMENT_3D('',#21610,#17143,#17144);
#14834=AXIS2_PLACEMENT_3D('',#21611,#17145,#17146);
#14835=AXIS2_PLACEMENT_3D('',#21617,#17150,#17151);
#14836=AXIS2_PLACEMENT_3D('',#21626,#17156,#17157);
#14837=AXIS2_PLACEMENT_3D('',#21632,#17161,#17162);
#14838=AXIS2_PLACEMENT_3D('',#21638,#17166,#17167);
#14839=AXIS2_PLACEMENT_3D('',#21641,#17170,#17171);
#14840=AXIS2_PLACEMENT_3D('',#21644,#17174,#17175);
#14841=AXIS2_PLACEMENT_3D('',#21645,#17176,#17177);
#14842=AXIS2_PLACEMENT_3D('',#21646,#17178,#17179);
#14843=AXIS2_PLACEMENT_3D('',#21647,#17180,#17181);
#14844=AXIS2_PLACEMENT_3D('',#21649,#17182,#17183);
#14845=AXIS2_PLACEMENT_3D('',#21652,#17185,#17186);
#14846=AXIS2_PLACEMENT_3D('',#21653,#17187,#17188);
#14847=AXIS2_PLACEMENT_3D('',#21655,#17189,#17190);
#14848=AXIS2_PLACEMENT_3D('',#21658,#17192,#17193);
#14849=AXIS2_PLACEMENT_3D('',#21659,#17194,#17195);
#14850=AXIS2_PLACEMENT_3D('',#21660,#17196,#17197);
#14851=AXIS2_PLACEMENT_3D('',#21661,#17198,#17199);
#14852=AXIS2_PLACEMENT_3D('',#21662,#17200,#17201);
#14853=AXIS2_PLACEMENT_3D('',#21664,#17202,#17203);
#14854=AXIS2_PLACEMENT_3D('',#21667,#17205,#17206);
#14855=AXIS2_PLACEMENT_3D('',#21668,#17207,#17208);
#14856=AXIS2_PLACEMENT_3D('',#21670,#17209,#17210);
#14857=AXIS2_PLACEMENT_3D('',#21673,#17212,#17213);
#14858=AXIS2_PLACEMENT_3D('',#21674,#17214,#17215);
#14859=AXIS2_PLACEMENT_3D('',#21675,#17216,#17217);
#14860=AXIS2_PLACEMENT_3D('',#21676,#17218,#17219);
#14861=AXIS2_PLACEMENT_3D('',#21677,#17220,#17221);
#14862=AXIS2_PLACEMENT_3D('',#21679,#17222,#17223);
#14863=AXIS2_PLACEMENT_3D('',#21682,#17225,#17226);
#14864=AXIS2_PLACEMENT_3D('',#21683,#17227,#17228);
#14865=AXIS2_PLACEMENT_3D('',#21685,#17229,#17230);
#14866=AXIS2_PLACEMENT_3D('',#21688,#17232,#17233);
#14867=AXIS2_PLACEMENT_3D('',#21689,#17234,#17235);
#14868=AXIS2_PLACEMENT_3D('',#21690,#17236,#17237);
#14869=AXIS2_PLACEMENT_3D('',#21691,#17238,#17239);
#14870=AXIS2_PLACEMENT_3D('',#21692,#17240,#17241);
#14871=AXIS2_PLACEMENT_3D('',#21694,#17242,#17243);
#14872=AXIS2_PLACEMENT_3D('',#21697,#17245,#17246);
#14873=AXIS2_PLACEMENT_3D('',#21698,#17247,#17248);
#14874=AXIS2_PLACEMENT_3D('',#21700,#17249,#17250);
#14875=AXIS2_PLACEMENT_3D('',#21703,#17252,#17253);
#14876=AXIS2_PLACEMENT_3D('',#21704,#17254,#17255);
#14877=AXIS2_PLACEMENT_3D('',#21705,#17256,#17257);
#14878=AXIS2_PLACEMENT_3D('',#21706,#17258,#17259);
#14879=AXIS2_PLACEMENT_3D('',#21707,#17260,#17261);
#14880=AXIS2_PLACEMENT_3D('',#21709,#17262,#17263);
#14881=AXIS2_PLACEMENT_3D('',#21712,#17265,#17266);
#14882=AXIS2_PLACEMENT_3D('',#21713,#17267,#17268);
#14883=AXIS2_PLACEMENT_3D('',#21715,#17269,#17270);
#14884=AXIS2_PLACEMENT_3D('',#21718,#17272,#17273);
#14885=AXIS2_PLACEMENT_3D('',#21719,#17274,#17275);
#14886=AXIS2_PLACEMENT_3D('',#21720,#17276,#17277);
#14887=AXIS2_PLACEMENT_3D('',#21721,#17278,#17279);
#14888=AXIS2_PLACEMENT_3D('',#21722,#17280,#17281);
#14889=AXIS2_PLACEMENT_3D('',#21727,#17283,#17284);
#14890=AXIS2_PLACEMENT_3D('',#21730,#17286,#17287);
#14891=AXIS2_PLACEMENT_3D('',#21731,#17288,#17289);
#14892=AXIS2_PLACEMENT_3D('',#21736,#17291,#17292);
#14893=AXIS2_PLACEMENT_3D('',#21739,#17294,#17295);
#14894=AXIS2_PLACEMENT_3D('',#21740,#17296,#17297);
#14895=AXIS2_PLACEMENT_3D('',#21745,#17299,#17300);
#14896=AXIS2_PLACEMENT_3D('',#21748,#17302,#17303);
#14897=AXIS2_PLACEMENT_3D('',#21749,#17304,#17305);
#14898=AXIS2_PLACEMENT_3D('',#21754,#17307,#17308);
#14899=AXIS2_PLACEMENT_3D('',#21757,#17310,#17311);
#14900=AXIS2_PLACEMENT_3D('',#21758,#17312,#17313);
#14901=AXIS2_PLACEMENT_3D('',#21759,#17314,#17315);
#14902=AXIS2_PLACEMENT_3D('',#21760,#17316,#17317);
#14903=AXIS2_PLACEMENT_3D('',#21761,#17318,#17319);
#14904=AXIS2_PLACEMENT_3D('',#21762,#17320,#17321);
#14905=AXIS2_PLACEMENT_3D('',#21764,#17322,#17323);
#14906=AXIS2_PLACEMENT_3D('',#21765,#17324,#17325);
#14907=AXIS2_PLACEMENT_3D('',#21766,#17326,#17327);
#14908=AXIS2_PLACEMENT_3D('',#21767,#17328,#17329);
#14909=AXIS2_PLACEMENT_3D('',#21768,#17330,#17331);
#14910=AXIS2_PLACEMENT_3D('',#21769,#17332,#17333);
#14911=AXIS2_PLACEMENT_3D('',#21770,#17334,#17335);
#14912=AXIS2_PLACEMENT_3D('',#21771,#17336,#17337);
#14913=AXIS2_PLACEMENT_3D('',#21772,#17338,#17339);
#14914=AXIS2_PLACEMENT_3D('',#21773,#17340,#17341);
#14915=AXIS2_PLACEMENT_3D('',#21775,#17342,#17343);
#14916=AXIS2_PLACEMENT_3D('',#21778,#17345,#17346);
#14917=AXIS2_PLACEMENT_3D('',#21779,#17347,#17348);
#14918=AXIS2_PLACEMENT_3D('',#21781,#17349,#17350);
#14919=AXIS2_PLACEMENT_3D('',#21782,#17351,#17352);
#14920=AXIS2_PLACEMENT_3D('',#21784,#17354,#17355);
#14921=AXIS2_PLACEMENT_3D('',#21785,#17356,#17357);
#14922=AXIS2_PLACEMENT_3D('',#21786,#17358,#17359);
#14923=AXIS2_PLACEMENT_3D('',#21791,#17361,#17362);
#14924=AXIS2_PLACEMENT_3D('',#21794,#17364,#17365);
#14925=AXIS2_PLACEMENT_3D('',#21795,#17366,#17367);
#14926=AXIS2_PLACEMENT_3D('',#21797,#17368,#17369);
#14927=AXIS2_PLACEMENT_3D('',#21799,#17370,#17371);
#14928=AXIS2_PLACEMENT_3D('',#21800,#17372,#17373);
#14929=AXIS2_PLACEMENT_3D('',#21801,#17374,#17375);
#14930=AXIS2_PLACEMENT_3D('',#21804,#17376,#17377);
#14931=AXIS2_PLACEMENT_3D('',#21806,#17378,#17379);
#14932=AXIS2_PLACEMENT_3D('',#21808,#17380,#17381);
#14933=AXIS2_PLACEMENT_3D('',#21809,#17382,#17383);
#14934=AXIS2_PLACEMENT_3D('',#21810,#17384,#17385);
#14935=AXIS2_PLACEMENT_3D('',#21814,#17387,#17388);
#14936=AXIS2_PLACEMENT_3D('',#21816,#17390,#17391);
#14937=AXIS2_PLACEMENT_3D('',#21819,#17392,#17393);
#14938=AXIS2_PLACEMENT_3D('',#21821,#17394,#17395);
#14939=AXIS2_PLACEMENT_3D('',#21823,#17396,#17397);
#14940=AXIS2_PLACEMENT_3D('',#21824,#17398,#17399);
#14941=AXIS2_PLACEMENT_3D('',#21825,#17400,#17401);
#14942=AXIS2_PLACEMENT_3D('',#21829,#17403,#17404);
#14943=AXIS2_PLACEMENT_3D('',#21831,#17406,#17407);
#14944=AXIS2_PLACEMENT_3D('',#21834,#17408,#17409);
#14945=AXIS2_PLACEMENT_3D('',#21836,#17410,#17411);
#14946=AXIS2_PLACEMENT_3D('',#21838,#17412,#17413);
#14947=AXIS2_PLACEMENT_3D('',#21839,#17414,#17415);
#14948=AXIS2_PLACEMENT_3D('',#21840,#17416,#17417);
#14949=AXIS2_PLACEMENT_3D('',#21844,#17419,#17420);
#14950=AXIS2_PLACEMENT_3D('',#21846,#17422,#17423);
#14951=AXIS2_PLACEMENT_3D('',#21850,#17425,#17426);
#14952=AXIS2_PLACEMENT_3D('',#21852,#17428,#17429);
#14953=AXIS2_PLACEMENT_3D('',#21856,#17431,#17432);
#14954=AXIS2_PLACEMENT_3D('',#21858,#17434,#17435);
#14955=AXIS2_PLACEMENT_3D('',#21862,#17437,#17438);
#14956=AXIS2_PLACEMENT_3D('',#21864,#17440,#17441);
#14957=AXIS2_PLACEMENT_3D('',#21865,#17442,#17443);
#14958=AXIS2_PLACEMENT_3D('',#21867,#17444,#17445);
#14959=AXIS2_PLACEMENT_3D('',#21869,#17447,#17448);
#14960=AXIS2_PLACEMENT_3D('',#21870,#17449,#17450);
#14961=AXIS2_PLACEMENT_3D('',#21871,#17451,#17452);
#14962=AXIS2_PLACEMENT_3D('',#21872,#17453,#17454);
#14963=AXIS2_PLACEMENT_3D('',#21874,#17455,#17456);
#14964=AXIS2_PLACEMENT_3D('',#21875,#17457,#17458);
#14965=AXIS2_PLACEMENT_3D('',#21877,#17459,#17460);
#14966=AXIS2_PLACEMENT_3D('',#21878,#17461,#17462);
#14967=AXIS2_PLACEMENT_3D('',#21879,#17463,#17464);
#14968=AXIS2_PLACEMENT_3D('',#21880,#17465,#17466);
#14969=AXIS2_PLACEMENT_3D('',#21882,#17467,#17468);
#14970=AXIS2_PLACEMENT_3D('',#21883,#17469,#17470);
#14971=AXIS2_PLACEMENT_3D('',#21884,#17471,#17472);
#14972=AXIS2_PLACEMENT_3D('',#21885,#17473,#17474);
#14973=AXIS2_PLACEMENT_3D('',#21887,#17476,#17477);
#14974=AXIS2_PLACEMENT_3D('',#21888,#17478,#17479);
#14975=AXIS2_PLACEMENT_3D('',#21890,#17481,#17482);
#14976=AXIS2_PLACEMENT_3D('',#21891,#17483,#17484);
#14977=AXIS2_PLACEMENT_3D('',#21900,#17489,#17490);
#14978=AXIS2_PLACEMENT_3D('',#21909,#17495,#17496);
#14979=AXIS2_PLACEMENT_3D('',#21914,#17498,#17499);
#14980=AXIS2_PLACEMENT_3D('',#21917,#17501,#17502);
#14981=AXIS2_PLACEMENT_3D('',#21918,#17503,#17504);
#14982=AXIS2_PLACEMENT_3D('',#21919,#17505,#17506);
#14983=AXIS2_PLACEMENT_3D('',#21920,#17507,#17508);
#14984=AXIS2_PLACEMENT_3D('',#21921,#17509,#17510);
#14985=AXIS2_PLACEMENT_3D('',#21922,#17511,#17512);
#14986=AXIS2_PLACEMENT_3D('',#21923,#17513,#17514);
#14987=AXIS2_PLACEMENT_3D('',#21924,#17515,#17516);
#14988=AXIS2_PLACEMENT_3D('',#21928,#17518,#17519);
#14989=AXIS2_PLACEMENT_3D('',#21930,#17521,#17522);
#14990=AXIS2_PLACEMENT_3D('',#21934,#17525,#17526);
#14991=AXIS2_PLACEMENT_3D('',#21938,#17529,#17530);
#14992=AXIS2_PLACEMENT_3D('',#21939,#17531,#17532);
#14993=AXIS2_PLACEMENT_3D('',#21940,#17533,#17534);
#14994=AXIS2_PLACEMENT_3D('',#21941,#17535,#17536);
#14995=AXIS2_PLACEMENT_3D('',#21942,#17537,#17538);
#14996=AXIS2_PLACEMENT_3D('',#21944,#17539,#17540);
#14997=AXIS2_PLACEMENT_3D('',#21947,#17542,#17543);
#14998=AXIS2_PLACEMENT_3D('',#21948,#17544,#17545);
#14999=AXIS2_PLACEMENT_3D('',#21950,#17546,#17547);
#15000=AXIS2_PLACEMENT_3D('',#21951,#17548,#17549);
#15001=AXIS2_PLACEMENT_3D('',#21953,#17550,#17551);
#15002=AXIS2_PLACEMENT_3D('',#21955,#17553,#17554);
#15003=AXIS2_PLACEMENT_3D('',#21957,#17555,#17556);
#15004=AXIS2_PLACEMENT_3D('',#21960,#17558,#17559);
#15005=AXIS2_PLACEMENT_3D('',#21961,#17560,#17561);
#15006=AXIS2_PLACEMENT_3D('',#21963,#17562,#17563);
#15007=AXIS2_PLACEMENT_3D('',#21964,#17564,#17565);
#15008=AXIS2_PLACEMENT_3D('',#21966,#17566,#17567);
#15009=AXIS2_PLACEMENT_3D('',#21968,#17569,#17570);
#15010=AXIS2_PLACEMENT_3D('',#21970,#17571,#17572);
#15011=AXIS2_PLACEMENT_3D('',#21973,#17574,#17575);
#15012=AXIS2_PLACEMENT_3D('',#21974,#17576,#17577);
#15013=AXIS2_PLACEMENT_3D('',#21976,#17578,#17579);
#15014=AXIS2_PLACEMENT_3D('',#21977,#17580,#17581);
#15015=AXIS2_PLACEMENT_3D('',#21979,#17582,#17583);
#15016=AXIS2_PLACEMENT_3D('',#21981,#17585,#17586);
#15017=AXIS2_PLACEMENT_3D('',#21983,#17587,#17588);
#15018=AXIS2_PLACEMENT_3D('',#21986,#17590,#17591);
#15019=AXIS2_PLACEMENT_3D('',#21987,#17592,#17593);
#15020=AXIS2_PLACEMENT_3D('',#21989,#17594,#17595);
#15021=AXIS2_PLACEMENT_3D('',#21990,#17596,#17597);
#15022=AXIS2_PLACEMENT_3D('',#21992,#17598,#17599);
#15023=AXIS2_PLACEMENT_3D('',#21994,#17601,#17602);
#15024=AXIS2_PLACEMENT_3D('',#21996,#17603,#17604);
#15025=AXIS2_PLACEMENT_3D('',#21999,#17606,#17607);
#15026=AXIS2_PLACEMENT_3D('',#22000,#17608,#17609);
#15027=AXIS2_PLACEMENT_3D('',#22001,#17610,#17611);
#15028=AXIS2_PLACEMENT_3D('',#22003,#17612,#17613);
#15029=AXIS2_PLACEMENT_3D('',#22006,#17615,#17616);
#15030=AXIS2_PLACEMENT_3D('',#22007,#17617,#17618);
#15031=AXIS2_PLACEMENT_3D('',#22008,#17619,#17620);
#15032=AXIS2_PLACEMENT_3D('',#22017,#17625,#17626);
#15033=AXIS2_PLACEMENT_3D('',#22023,#17630,#17631);
#15034=AXIS2_PLACEMENT_3D('',#22029,#17635,#17636);
#15035=AXIS2_PLACEMENT_3D('',#22032,#17639,#17640);
#15036=AXIS2_PLACEMENT_3D('',#22033,#17641,#17642);
#15037=AXIS2_PLACEMENT_3D('',#22034,#17643,#17644);
#15038=AXIS2_PLACEMENT_3D('',#22035,#17645,#17646);
#15039=AXIS2_PLACEMENT_3D('',#22037,#17647,#17648);
#15040=AXIS2_PLACEMENT_3D('',#22040,#17650,#17651);
#15041=AXIS2_PLACEMENT_3D('',#22041,#17652,#17653);
#15042=AXIS2_PLACEMENT_3D('',#22043,#17654,#17655);
#15043=AXIS2_PLACEMENT_3D('',#22046,#17657,#17658);
#15044=AXIS2_PLACEMENT_3D('',#22047,#17659,#17660);
#15045=AXIS2_PLACEMENT_3D('',#22048,#17661,#17662);
#15046=AXIS2_PLACEMENT_3D('',#22049,#17663,#17664);
#15047=AXIS2_PLACEMENT_3D('',#22050,#17665,#17666);
#15048=AXIS2_PLACEMENT_3D('',#22052,#17667,#17668);
#15049=AXIS2_PLACEMENT_3D('',#22055,#17670,#17671);
#15050=AXIS2_PLACEMENT_3D('',#22056,#17672,#17673);
#15051=AXIS2_PLACEMENT_3D('',#22058,#17674,#17675);
#15052=AXIS2_PLACEMENT_3D('',#22061,#17677,#17678);
#15053=AXIS2_PLACEMENT_3D('',#22062,#17679,#17680);
#15054=AXIS2_PLACEMENT_3D('',#22063,#17681,#17682);
#15055=AXIS2_PLACEMENT_3D('',#22064,#17683,#17684);
#15056=AXIS2_PLACEMENT_3D('',#22065,#17685,#17686);
#15057=AXIS2_PLACEMENT_3D('',#22067,#17687,#17688);
#15058=AXIS2_PLACEMENT_3D('',#22070,#17690,#17691);
#15059=AXIS2_PLACEMENT_3D('',#22071,#17692,#17693);
#15060=AXIS2_PLACEMENT_3D('',#22073,#17694,#17695);
#15061=AXIS2_PLACEMENT_3D('',#22074,#17696,#17697);
#15062=AXIS2_PLACEMENT_3D('',#22076,#17698,#17699);
#15063=AXIS2_PLACEMENT_3D('',#22078,#17701,#17702);
#15064=AXIS2_PLACEMENT_3D('',#22080,#17703,#17704);
#15065=AXIS2_PLACEMENT_3D('',#22083,#17706,#17707);
#15066=AXIS2_PLACEMENT_3D('',#22084,#17708,#17709);
#15067=AXIS2_PLACEMENT_3D('',#22086,#17710,#17711);
#15068=AXIS2_PLACEMENT_3D('',#22087,#17712,#17713);
#15069=AXIS2_PLACEMENT_3D('',#22089,#17714,#17715);
#15070=AXIS2_PLACEMENT_3D('',#22091,#17717,#17718);
#15071=AXIS2_PLACEMENT_3D('',#22093,#17719,#17720);
#15072=AXIS2_PLACEMENT_3D('',#22096,#17722,#17723);
#15073=AXIS2_PLACEMENT_3D('',#22097,#17724,#17725);
#15074=AXIS2_PLACEMENT_3D('',#22099,#17726,#17727);
#15075=AXIS2_PLACEMENT_3D('',#22100,#17728,#17729);
#15076=AXIS2_PLACEMENT_3D('',#22102,#17730,#17731);
#15077=AXIS2_PLACEMENT_3D('',#22104,#17733,#17734);
#15078=AXIS2_PLACEMENT_3D('',#22106,#17735,#17736);
#15079=AXIS2_PLACEMENT_3D('',#22109,#17738,#17739);
#15080=AXIS2_PLACEMENT_3D('',#22110,#17740,#17741);
#15081=AXIS2_PLACEMENT_3D('',#22112,#17742,#17743);
#15082=AXIS2_PLACEMENT_3D('',#22113,#17744,#17745);
#15083=AXIS2_PLACEMENT_3D('',#22115,#17746,#17747);
#15084=AXIS2_PLACEMENT_3D('',#22117,#17749,#17750);
#15085=AXIS2_PLACEMENT_3D('',#22119,#17751,#17752);
#15086=AXIS2_PLACEMENT_3D('',#22122,#17754,#17755);
#15087=AXIS2_PLACEMENT_3D('',#22123,#17756,#17757);
#15088=AXIS2_PLACEMENT_3D('',#22124,#17758,#17759);
#15089=AXIS2_PLACEMENT_3D('',#22126,#17760,#17761);
#15090=AXIS2_PLACEMENT_3D('',#22129,#17763,#17764);
#15091=AXIS2_PLACEMENT_3D('',#22130,#17765,#17766);
#15092=AXIS2_PLACEMENT_3D('',#22131,#17767,#17768);
#15093=AXIS2_PLACEMENT_3D('',#22140,#17773,#17774);
#15094=AXIS2_PLACEMENT_3D('',#22146,#17778,#17779);
#15095=AXIS2_PLACEMENT_3D('',#22152,#17783,#17784);
#15096=AXIS2_PLACEMENT_3D('',#22155,#17787,#17788);
#15097=AXIS2_PLACEMENT_3D('',#22156,#17789,#17790);
#15098=AXIS2_PLACEMENT_3D('',#22157,#17791,#17792);
#15099=AXIS2_PLACEMENT_3D('',#22158,#17793,#17794);
#15100=AXIS2_PLACEMENT_3D('',#22160,#17795,#17796);
#15101=AXIS2_PLACEMENT_3D('',#22163,#17798,#17799);
#15102=AXIS2_PLACEMENT_3D('',#22164,#17800,#17801);
#15103=AXIS2_PLACEMENT_3D('',#22166,#17802,#17803);
#15104=AXIS2_PLACEMENT_3D('',#22169,#17805,#17806);
#15105=AXIS2_PLACEMENT_3D('',#22170,#17807,#17808);
#15106=AXIS2_PLACEMENT_3D('',#22171,#17809,#17810);
#15107=AXIS2_PLACEMENT_3D('',#22172,#17811,#17812);
#15108=AXIS2_PLACEMENT_3D('',#22173,#17813,#17814);
#15109=AXIS2_PLACEMENT_3D('',#22175,#17815,#17816);
#15110=AXIS2_PLACEMENT_3D('',#22178,#17818,#17819);
#15111=AXIS2_PLACEMENT_3D('',#22179,#17820,#17821);
#15112=AXIS2_PLACEMENT_3D('',#22181,#17822,#17823);
#15113=AXIS2_PLACEMENT_3D('',#22184,#17825,#17826);
#15114=AXIS2_PLACEMENT_3D('',#22185,#17827,#17828);
#15115=AXIS2_PLACEMENT_3D('',#22186,#17829,#17830);
#15116=AXIS2_PLACEMENT_3D('',#22187,#17831,#17832);
#15117=AXIS2_PLACEMENT_3D('',#22188,#17833,#17834);
#15118=AXIS2_PLACEMENT_3D('',#22190,#17835,#17836);
#15119=AXIS2_PLACEMENT_3D('',#22193,#17838,#17839);
#15120=AXIS2_PLACEMENT_3D('',#22194,#17840,#17841);
#15121=AXIS2_PLACEMENT_3D('',#22196,#17842,#17843);
#15122=AXIS2_PLACEMENT_3D('',#22197,#17844,#17845);
#15123=AXIS2_PLACEMENT_3D('',#22199,#17846,#17847);
#15124=AXIS2_PLACEMENT_3D('',#22201,#17849,#17850);
#15125=AXIS2_PLACEMENT_3D('',#22203,#17851,#17852);
#15126=AXIS2_PLACEMENT_3D('',#22206,#17854,#17855);
#15127=AXIS2_PLACEMENT_3D('',#22207,#17856,#17857);
#15128=AXIS2_PLACEMENT_3D('',#22209,#17858,#17859);
#15129=AXIS2_PLACEMENT_3D('',#22210,#17860,#17861);
#15130=AXIS2_PLACEMENT_3D('',#22212,#17862,#17863);
#15131=AXIS2_PLACEMENT_3D('',#22214,#17865,#17866);
#15132=AXIS2_PLACEMENT_3D('',#22223,#17871,#17872);
#15133=AXIS2_PLACEMENT_3D('',#22229,#17876,#17877);
#15134=AXIS2_PLACEMENT_3D('',#22235,#17881,#17882);
#15135=AXIS2_PLACEMENT_3D('',#22238,#17885,#17886);
#15136=AXIS2_PLACEMENT_3D('',#22239,#17887,#17888);
#15137=AXIS2_PLACEMENT_3D('',#22240,#17889,#17890);
#15138=AXIS2_PLACEMENT_3D('',#22241,#17891,#17892);
#15139=AXIS2_PLACEMENT_3D('',#22250,#17897,#17898);
#15140=AXIS2_PLACEMENT_3D('',#22256,#17902,#17903);
#15141=AXIS2_PLACEMENT_3D('',#22262,#17907,#17908);
#15142=AXIS2_PLACEMENT_3D('',#22265,#17911,#17912);
#15143=AXIS2_PLACEMENT_3D('',#22266,#17913,#17914);
#15144=AXIS2_PLACEMENT_3D('',#22267,#17915,#17916);
#15145=AXIS2_PLACEMENT_3D('',#22268,#17917,#17918);
#15146=AXIS2_PLACEMENT_3D('',#22270,#17919,#17920);
#15147=AXIS2_PLACEMENT_3D('',#22273,#17922,#17923);
#15148=AXIS2_PLACEMENT_3D('',#22274,#17924,#17925);
#15149=AXIS2_PLACEMENT_3D('',#22276,#17926,#17927);
#15150=AXIS2_PLACEMENT_3D('',#22279,#17929,#17930);
#15151=AXIS2_PLACEMENT_3D('',#22280,#17931,#17932);
#15152=AXIS2_PLACEMENT_3D('',#22289,#17937,#17938);
#15153=AXIS2_PLACEMENT_3D('',#22295,#17942,#17943);
#15154=AXIS2_PLACEMENT_3D('',#22301,#17947,#17948);
#15155=AXIS2_PLACEMENT_3D('',#22304,#17951,#17952);
#15156=AXIS2_PLACEMENT_3D('',#22305,#17953,#17954);
#15157=AXIS2_PLACEMENT_3D('',#22306,#17955,#17956);
#15158=AXIS2_PLACEMENT_3D('',#22307,#17957,#17958);
#15159=AXIS2_PLACEMENT_3D('',#22309,#17959,#17960);
#15160=AXIS2_PLACEMENT_3D('',#22312,#17962,#17963);
#15161=AXIS2_PLACEMENT_3D('',#22313,#17964,#17965);
#15162=AXIS2_PLACEMENT_3D('',#22315,#17966,#17967);
#15163=AXIS2_PLACEMENT_3D('',#22318,#17969,#17970);
#15164=AXIS2_PLACEMENT_3D('',#22319,#17971,#17972);
#15165=AXIS2_PLACEMENT_3D('',#22328,#17977,#17978);
#15166=AXIS2_PLACEMENT_3D('',#22334,#17982,#17983);
#15167=AXIS2_PLACEMENT_3D('',#22340,#17987,#17988);
#15168=AXIS2_PLACEMENT_3D('',#22343,#17991,#17992);
#15169=AXIS2_PLACEMENT_3D('',#22344,#17993,#17994);
#15170=AXIS2_PLACEMENT_3D('',#22345,#17995,#17996);
#15171=AXIS2_PLACEMENT_3D('',#22346,#17997,#17998);
#15172=AXIS2_PLACEMENT_3D('',#22348,#17999,#18000);
#15173=AXIS2_PLACEMENT_3D('',#22351,#18002,#18003);
#15174=AXIS2_PLACEMENT_3D('',#22352,#18004,#18005);
#15175=AXIS2_PLACEMENT_3D('',#22354,#18006,#18007);
#15176=AXIS2_PLACEMENT_3D('',#22357,#18009,#18010);
#15177=AXIS2_PLACEMENT_3D('',#22358,#18011,#18012);
#15178=AXIS2_PLACEMENT_3D('',#22360,#18013,#18014);
#15179=AXIS2_PLACEMENT_3D('',#22363,#18016,#18017);
#15180=AXIS2_PLACEMENT_3D('',#22364,#18018,#18019);
#15181=AXIS2_PLACEMENT_3D('',#22366,#18020,#18021);
#15182=AXIS2_PLACEMENT_3D('',#22369,#18023,#18024);
#15183=AXIS2_PLACEMENT_3D('',#22370,#18025,#18026);
#15184=AXIS2_PLACEMENT_3D('',#22379,#18031,#18032);
#15185=AXIS2_PLACEMENT_3D('',#22385,#18036,#18037);
#15186=AXIS2_PLACEMENT_3D('',#22391,#18041,#18042);
#15187=AXIS2_PLACEMENT_3D('',#22394,#18045,#18046);
#15188=AXIS2_PLACEMENT_3D('',#22395,#18047,#18048);
#15189=AXIS2_PLACEMENT_3D('',#22396,#18049,#18050);
#15190=AXIS2_PLACEMENT_3D('',#22397,#18051,#18052);
#15191=AXIS2_PLACEMENT_3D('',#22398,#18053,#18054);
#15192=AXIS2_PLACEMENT_3D('',#22401,#18055,#18056);
#15193=AXIS2_PLACEMENT_3D('',#22402,#18057,#18058);
#15194=AXIS2_PLACEMENT_3D('',#22404,#18059,#18060);
#15195=AXIS2_PLACEMENT_3D('',#22406,#18061,#18062);
#15196=AXIS2_PLACEMENT_3D('',#22407,#18063,#18064);
#15197=AXIS2_PLACEMENT_3D('',#22408,#18065,#18066);
#15198=AXIS2_PLACEMENT_3D('',#22411,#18068,#18069);
#15199=AXIS2_PLACEMENT_3D('',#22412,#18070,#18071);
#15200=AXIS2_PLACEMENT_3D('',#22414,#18072,#18073);
#15201=AXIS2_PLACEMENT_3D('',#22417,#18075,#18076);
#15202=AXIS2_PLACEMENT_3D('',#22418,#18077,#18078);
#15203=AXIS2_PLACEMENT_3D('',#22421,#18080,#18081);
#15204=AXIS2_PLACEMENT_3D('',#22422,#18082,#18083);
#15205=AXIS2_PLACEMENT_3D('',#22423,#18084,#18085);
#15206=AXIS2_PLACEMENT_3D('',#22425,#18086,#18087);
#15207=AXIS2_PLACEMENT_3D('',#22427,#18089,#18090);
#15208=AXIS2_PLACEMENT_3D('',#22429,#18091,#18092);
#15209=AXIS2_PLACEMENT_3D('',#22430,#18093,#18094);
#15210=AXIS2_PLACEMENT_3D('',#22432,#18096,#18097);
#15211=AXIS2_PLACEMENT_3D('',#22433,#18098,#18099);
#15212=AXIS2_PLACEMENT_3D('',#22436,#18100,#18101);
#15213=AXIS2_PLACEMENT_3D('',#22437,#18102,#18103);
#15214=AXIS2_PLACEMENT_3D('',#22439,#18104,#18105);
#15215=AXIS2_PLACEMENT_3D('',#22441,#18106,#18107);
#15216=AXIS2_PLACEMENT_3D('',#22442,#18108,#18109);
#15217=AXIS2_PLACEMENT_3D('',#22443,#18110,#18111);
#15218=AXIS2_PLACEMENT_3D('',#22445,#18112,#18113);
#15219=AXIS2_PLACEMENT_3D('',#22447,#18115,#18116);
#15220=AXIS2_PLACEMENT_3D('',#22449,#18117,#18118);
#15221=AXIS2_PLACEMENT_3D('',#22451,#18119,#18120);
#15222=AXIS2_PLACEMENT_3D('',#22452,#18121,#18122);
#15223=AXIS2_PLACEMENT_3D('',#22454,#18123,#18124);
#15224=AXIS2_PLACEMENT_3D('',#22456,#18126,#18127);
#15225=AXIS2_PLACEMENT_3D('',#22458,#18128,#18129);
#15226=AXIS2_PLACEMENT_3D('',#22460,#18131,#18132);
#15227=AXIS2_PLACEMENT_3D('',#22462,#18133,#18134);
#15228=AXIS2_PLACEMENT_3D('',#22464,#18136,#18137);
#15229=AXIS2_PLACEMENT_3D('',#22465,#18138,#18139);
#15230=AXIS2_PLACEMENT_3D('',#22467,#18141,#18142);
#15231=AXIS2_PLACEMENT_3D('',#22468,#18143,#18144);
#15232=AXIS2_PLACEMENT_3D('',#22471,#18145,#18146);
#15233=AXIS2_PLACEMENT_3D('',#22472,#18147,#18148);
#15234=AXIS2_PLACEMENT_3D('',#22475,#18149,#18150);
#15235=AXIS2_PLACEMENT_3D('',#22476,#18151,#18152);
#15236=AXIS2_PLACEMENT_3D('',#22479,#18153,#18154);
#15237=AXIS2_PLACEMENT_3D('',#22480,#18155,#18156);
#15238=AXIS2_PLACEMENT_3D('',#22483,#18157,#18158);
#15239=AXIS2_PLACEMENT_3D('',#22484,#18159,#18160);
#15240=AXIS2_PLACEMENT_3D('',#22487,#18161,#18162);
#15241=AXIS2_PLACEMENT_3D('',#22488,#18163,#18164);
#15242=AXIS2_PLACEMENT_3D('',#22491,#18165,#18166);
#15243=AXIS2_PLACEMENT_3D('',#22492,#18167,#18168);
#15244=AXIS2_PLACEMENT_3D('',#22495,#18169,#18170);
#15245=AXIS2_PLACEMENT_3D('',#22496,#18171,#18172);
#15246=AXIS2_PLACEMENT_3D('',#22499,#18173,#18174);
#15247=AXIS2_PLACEMENT_3D('',#22500,#18175,#18176);
#15248=AXIS2_PLACEMENT_3D('',#22501,#18177,#18178);
#15249=AXIS2_PLACEMENT_3D('',#22527,#18179,#18180);
#15250=AXIS2_PLACEMENT_3D('',#22551,#18181,#18182);
#15251=AXIS2_PLACEMENT_3D('',#22552,#18183,#18184);
#15252=AXIS2_PLACEMENT_3D('',#22554,#18185,#18186);
#15253=AXIS2_PLACEMENT_3D('',#22579,#18187,#18188);
#15254=AXIS2_PLACEMENT_3D('',#22604,#18189,#18190);
#15255=AXIS2_PLACEMENT_3D('',#22620,#18192,#18193);
#15256=AXIS2_PLACEMENT_3D('',#22635,#18194,#18195);
#15257=AXIS2_PLACEMENT_3D('',#22660,#18196,#18197);
#15258=AXIS2_PLACEMENT_3D('',#22685,#18198,#18199);
#15259=AXIS2_PLACEMENT_3D('',#22710,#18200,#18201);
#15260=AXIS2_PLACEMENT_3D('',#22734,#18202,#18203);
#15261=AXIS2_PLACEMENT_3D('',#22735,#18204,#18205);
#15262=AXIS2_PLACEMENT_3D('',#22737,#18206,#18207);
#15263=AXIS2_PLACEMENT_3D('',#22738,#18208,#18209);
#15264=AXIS2_PLACEMENT_3D('',#22739,#18210,#18211);
#15265=AXIS2_PLACEMENT_3D('',#22763,#18212,#18213);
#15266=AXIS2_PLACEMENT_3D('',#22764,#18214,#18215);
#15267=AXIS2_PLACEMENT_3D('',#22766,#18216,#18217);
#15268=AXIS2_PLACEMENT_3D('',#22767,#18218,#18219);
#15269=AXIS2_PLACEMENT_3D('',#22768,#18220,#18221);
#15270=AXIS2_PLACEMENT_3D('',#22792,#18222,#18223);
#15271=AXIS2_PLACEMENT_3D('',#22793,#18224,#18225);
#15272=AXIS2_PLACEMENT_3D('',#22795,#18226,#18227);
#15273=AXIS2_PLACEMENT_3D('',#22796,#18228,#18229);
#15274=AXIS2_PLACEMENT_3D('',#22797,#18230,#18231);
#15275=AXIS2_PLACEMENT_3D('',#22812,#18232,#18233);
#15276=AXIS2_PLACEMENT_3D('',#22825,#18234,#18235);
#15277=AXIS2_PLACEMENT_3D('',#22827,#18236,#18237);
#15278=AXIS2_PLACEMENT_3D('',#22828,#18238,#18239);
#15279=AXIS2_PLACEMENT_3D('',#22829,#18240,#18241);
#15280=AXIS2_PLACEMENT_3D('',#22853,#18242,#18243);
#15281=AXIS2_PLACEMENT_3D('',#22854,#18244,#18245);
#15282=AXIS2_PLACEMENT_3D('',#22856,#18246,#18247);
#15283=AXIS2_PLACEMENT_3D('',#22857,#18248,#18249);
#15284=AXIS2_PLACEMENT_3D('',#22858,#18250,#18251);
#15285=AXIS2_PLACEMENT_3D('',#22882,#18252,#18253);
#15286=AXIS2_PLACEMENT_3D('',#22883,#18254,#18255);
#15287=AXIS2_PLACEMENT_3D('',#22885,#18256,#18257);
#15288=AXIS2_PLACEMENT_3D('',#22886,#18258,#18259);
#15289=AXIS2_PLACEMENT_3D('',#22887,#18260,#18261);
#15290=AXIS2_PLACEMENT_3D('',#22911,#18262,#18263);
#15291=AXIS2_PLACEMENT_3D('',#22912,#18264,#18265);
#15292=AXIS2_PLACEMENT_3D('',#22914,#18266,#18267);
#15293=AXIS2_PLACEMENT_3D('',#22917,#18269,#18270);
#15294=AXIS2_PLACEMENT_3D('',#22941,#18271,#18272);
#15295=AXIS2_PLACEMENT_3D('',#22942,#18273,#18274);
#15296=AXIS2_PLACEMENT_3D('',#22943,#18275,#18276);
#15297=AXIS2_PLACEMENT_3D('',#22944,#18277,#18278);
#15298=AXIS2_PLACEMENT_3D('',#22945,#18279,#18280);
#15299=AXIS2_PLACEMENT_3D('',#22946,#18281,#18282);
#15300=AXIS2_PLACEMENT_3D('',#22947,#18283,#18284);
#15301=AXIS2_PLACEMENT_3D('',#22948,#18285,#18286);
#15302=AXIS2_PLACEMENT_3D('',#22949,#18287,#18288);
#15303=AXIS2_PLACEMENT_3D('',#22951,#18289,#18290);
#15304=AXIS2_PLACEMENT_3D('',#22953,#18291,#18292);
#15305=AXIS2_PLACEMENT_3D('',#22954,#18293,#18294);
#15306=AXIS2_PLACEMENT_3D('',#22956,#18295,#18296);
#15307=AXIS2_PLACEMENT_3D('',#22958,#18298,#18299);
#15308=AXIS2_PLACEMENT_3D('',#22960,#18300,#18301);
#15309=AXIS2_PLACEMENT_3D('',#22961,#18302,#18303);
#15310=AXIS2_PLACEMENT_3D('',#22963,#18305,#18306);
#15311=AXIS2_PLACEMENT_3D('',#22965,#18307,#18308);
#15312=AXIS2_PLACEMENT_3D('',#22967,#18309,#18310);
#15313=AXIS2_PLACEMENT_3D('',#22968,#18311,#18312);
#15314=AXIS2_PLACEMENT_3D('',#22970,#18313,#18314);
#15315=AXIS2_PLACEMENT_3D('',#22972,#18316,#18317);
#15316=AXIS2_PLACEMENT_3D('',#22974,#18318,#18319);
#15317=AXIS2_PLACEMENT_3D('',#22975,#18320,#18321);
#15318=AXIS2_PLACEMENT_3D('',#22977,#18323,#18324);
#15319=AXIS2_PLACEMENT_3D('',#22978,#18325,#18326);
#15320=AXIS2_PLACEMENT_3D('',#22979,#18327,#18328);
#15321=AXIS2_PLACEMENT_3D('',#22980,#18329,#18330);
#15322=AXIS2_PLACEMENT_3D('',#22981,#18331,#18332);
#15323=AXIS2_PLACEMENT_3D('',#22982,#18333,#18334);
#15324=AXIS2_PLACEMENT_3D('',#22983,#18335,#18336);
#15325=AXIS2_PLACEMENT_3D('',#22992,#18341,#18342);
#15326=AXIS2_PLACEMENT_3D('',#22998,#18346,#18347);
#15327=AXIS2_PLACEMENT_3D('',#23004,#18351,#18352);
#15328=AXIS2_PLACEMENT_3D('',#23010,#18356,#18357);
#15329=AXIS2_PLACEMENT_3D('',#23016,#18361,#18362);
#15330=AXIS2_PLACEMENT_3D('',#23019,#18365,#18366);
#15331=AXIS2_PLACEMENT_3D('',#23020,#18367,#18368);
#15332=AXIS2_PLACEMENT_3D('',#23021,#18369,#18370);
#15333=AXIS2_PLACEMENT_3D('',#23023,#18371,#18372);
#15334=AXIS2_PLACEMENT_3D('',#23025,#18373,#18374);
#15335=AXIS2_PLACEMENT_3D('',#23026,#18375,#18376);
#15336=AXIS2_PLACEMENT_3D('',#23029,#18378,#18379);
#15337=AXIS2_PLACEMENT_3D('',#23030,#18380,#18381);
#15338=AXIS2_PLACEMENT_3D('',#23031,#18382,#18383);
#15339=AXIS2_PLACEMENT_3D('',#23033,#18384,#18385);
#15340=AXIS2_PLACEMENT_3D('',#23034,#18386,#18387);
#15341=AXIS2_PLACEMENT_3D('',#23036,#18388,#18389);
#15342=AXIS2_PLACEMENT_3D('',#23038,#18391,#18392);
#15343=AXIS2_PLACEMENT_3D('',#23040,#18393,#18394);
#15344=AXIS2_PLACEMENT_3D('',#23042,#18396,#18397);
#15345=AXIS2_PLACEMENT_3D('',#23044,#18398,#18399);
#15346=AXIS2_PLACEMENT_3D('',#23046,#18401,#18402);
#15347=AXIS2_PLACEMENT_3D('',#23048,#18403,#18404);
#15348=AXIS2_PLACEMENT_3D('',#23049,#18405,#18406);
#15349=AXIS2_PLACEMENT_3D('',#23051,#18407,#18408);
#15350=AXIS2_PLACEMENT_3D('',#23053,#18410,#18411);
#15351=AXIS2_PLACEMENT_3D('',#23055,#18412,#18413);
#15352=AXIS2_PLACEMENT_3D('',#23057,#18415,#18416);
#15353=AXIS2_PLACEMENT_3D('',#23059,#18418,#18419);
#15354=AXIS2_PLACEMENT_3D('',#23060,#18420,#18421);
#15355=AXIS2_PLACEMENT_3D('',#23061,#18422,#18423);
#15356=AXIS2_PLACEMENT_3D('',#23064,#18424,#18425);
#15357=AXIS2_PLACEMENT_3D('',#23065,#18426,#18427);
#15358=AXIS2_PLACEMENT_3D('',#23067,#18428,#18429);
#15359=AXIS2_PLACEMENT_3D('',#23069,#18430,#18431);
#15360=AXIS2_PLACEMENT_3D('',#23070,#18432,#18433);
#15361=AXIS2_PLACEMENT_3D('',#23071,#18434,#18435);
#15362=AXIS2_PLACEMENT_3D('',#23074,#18437,#18438);
#15363=AXIS2_PLACEMENT_3D('',#23075,#18439,#18440);
#15364=AXIS2_PLACEMENT_3D('',#23077,#18441,#18442);
#15365=AXIS2_PLACEMENT_3D('',#23080,#18444,#18445);
#15366=AXIS2_PLACEMENT_3D('',#23081,#18446,#18447);
#15367=AXIS2_PLACEMENT_3D('',#23084,#18449,#18450);
#15368=AXIS2_PLACEMENT_3D('',#23085,#18451,#18452);
#15369=AXIS2_PLACEMENT_3D('',#23086,#18453,#18454);
#15370=AXIS2_PLACEMENT_3D('',#23088,#18455,#18456);
#15371=AXIS2_PLACEMENT_3D('',#23090,#18458,#18459);
#15372=AXIS2_PLACEMENT_3D('',#23092,#18460,#18461);
#15373=AXIS2_PLACEMENT_3D('',#23093,#18462,#18463);
#15374=AXIS2_PLACEMENT_3D('',#23095,#18465,#18466);
#15375=AXIS2_PLACEMENT_3D('',#23096,#18467,#18468);
#15376=AXIS2_PLACEMENT_3D('',#23099,#18469,#18470);
#15377=AXIS2_PLACEMENT_3D('',#23100,#18471,#18472);
#15378=AXIS2_PLACEMENT_3D('',#23102,#18473,#18474);
#15379=AXIS2_PLACEMENT_3D('',#23104,#18475,#18476);
#15380=AXIS2_PLACEMENT_3D('',#23105,#18477,#18478);
#15381=AXIS2_PLACEMENT_3D('',#23106,#18479,#18480);
#15382=AXIS2_PLACEMENT_3D('',#23108,#18481,#18482);
#15383=AXIS2_PLACEMENT_3D('',#23110,#18484,#18485);
#15384=AXIS2_PLACEMENT_3D('',#23112,#18486,#18487);
#15385=AXIS2_PLACEMENT_3D('',#23114,#18488,#18489);
#15386=AXIS2_PLACEMENT_3D('',#23115,#18490,#18491);
#15387=AXIS2_PLACEMENT_3D('',#23117,#18492,#18493);
#15388=AXIS2_PLACEMENT_3D('',#23119,#18495,#18496);
#15389=AXIS2_PLACEMENT_3D('',#23121,#18497,#18498);
#15390=AXIS2_PLACEMENT_3D('',#23123,#18500,#18501);
#15391=AXIS2_PLACEMENT_3D('',#23125,#18502,#18503);
#15392=AXIS2_PLACEMENT_3D('',#23127,#18505,#18506);
#15393=AXIS2_PLACEMENT_3D('',#23128,#18507,#18508);
#15394=AXIS2_PLACEMENT_3D('',#23130,#18510,#18511);
#15395=AXIS2_PLACEMENT_3D('',#23131,#18512,#18513);
#15396=AXIS2_PLACEMENT_3D('',#23134,#18514,#18515);
#15397=AXIS2_PLACEMENT_3D('',#23135,#18516,#18517);
#15398=AXIS2_PLACEMENT_3D('',#23138,#18518,#18519);
#15399=AXIS2_PLACEMENT_3D('',#23139,#18520,#18521);
#15400=AXIS2_PLACEMENT_3D('',#23142,#18522,#18523);
#15401=AXIS2_PLACEMENT_3D('',#23143,#18524,#18525);
#15402=AXIS2_PLACEMENT_3D('',#23146,#18526,#18527);
#15403=AXIS2_PLACEMENT_3D('',#23147,#18528,#18529);
#15404=AXIS2_PLACEMENT_3D('',#23150,#18530,#18531);
#15405=AXIS2_PLACEMENT_3D('',#23151,#18532,#18533);
#15406=AXIS2_PLACEMENT_3D('',#23154,#18534,#18535);
#15407=AXIS2_PLACEMENT_3D('',#23155,#18536,#18537);
#15408=AXIS2_PLACEMENT_3D('',#23158,#18538,#18539);
#15409=AXIS2_PLACEMENT_3D('',#23159,#18540,#18541);
#15410=AXIS2_PLACEMENT_3D('',#23160,#18542,#18543);
#15411=AXIS2_PLACEMENT_3D('',#23186,#18544,#18545);
#15412=AXIS2_PLACEMENT_3D('',#23210,#18546,#18547);
#15413=AXIS2_PLACEMENT_3D('',#23211,#18548,#18549);
#15414=AXIS2_PLACEMENT_3D('',#23213,#18550,#18551);
#15415=AXIS2_PLACEMENT_3D('',#23238,#18552,#18553);
#15416=AXIS2_PLACEMENT_3D('',#23263,#18554,#18555);
#15417=AXIS2_PLACEMENT_3D('',#23266,#18557,#18558);
#15418=AXIS2_PLACEMENT_3D('',#23268,#18559,#18560);
#15419=AXIS2_PLACEMENT_3D('',#23293,#18561,#18562);
#15420=AXIS2_PLACEMENT_3D('',#23318,#18563,#18564);
#15421=AXIS2_PLACEMENT_3D('',#23343,#18565,#18566);
#15422=AXIS2_PLACEMENT_3D('',#23367,#18567,#18568);
#15423=AXIS2_PLACEMENT_3D('',#23368,#18569,#18570);
#15424=AXIS2_PLACEMENT_3D('',#23370,#18571,#18572);
#15425=AXIS2_PLACEMENT_3D('',#23371,#18573,#18574);
#15426=AXIS2_PLACEMENT_3D('',#23372,#18575,#18576);
#15427=AXIS2_PLACEMENT_3D('',#23396,#18577,#18578);
#15428=AXIS2_PLACEMENT_3D('',#23397,#18579,#18580);
#15429=AXIS2_PLACEMENT_3D('',#23399,#18581,#18582);
#15430=AXIS2_PLACEMENT_3D('',#23400,#18583,#18584);
#15431=AXIS2_PLACEMENT_3D('',#23401,#18585,#18586);
#15432=AXIS2_PLACEMENT_3D('',#23425,#18587,#18588);
#15433=AXIS2_PLACEMENT_3D('',#23426,#18589,#18590);
#15434=AXIS2_PLACEMENT_3D('',#23428,#18591,#18592);
#15435=AXIS2_PLACEMENT_3D('',#23430,#18593,#18594);
#15436=AXIS2_PLACEMENT_3D('',#23431,#18595,#18596);
#15437=AXIS2_PLACEMENT_3D('',#23432,#18597,#18598);
#15438=AXIS2_PLACEMENT_3D('',#23456,#18599,#18600);
#15439=AXIS2_PLACEMENT_3D('',#23457,#18601,#18602);
#15440=AXIS2_PLACEMENT_3D('',#23459,#18603,#18604);
#15441=AXIS2_PLACEMENT_3D('',#23460,#18605,#18606);
#15442=AXIS2_PLACEMENT_3D('',#23461,#18607,#18608);
#15443=AXIS2_PLACEMENT_3D('',#23485,#18609,#18610);
#15444=AXIS2_PLACEMENT_3D('',#23486,#18611,#18612);
#15445=AXIS2_PLACEMENT_3D('',#23488,#18613,#18614);
#15446=AXIS2_PLACEMENT_3D('',#23489,#18615,#18616);
#15447=AXIS2_PLACEMENT_3D('',#23490,#18617,#18618);
#15448=AXIS2_PLACEMENT_3D('',#23514,#18619,#18620);
#15449=AXIS2_PLACEMENT_3D('',#23515,#18621,#18622);
#15450=AXIS2_PLACEMENT_3D('',#23517,#18623,#18624);
#15451=AXIS2_PLACEMENT_3D('',#23520,#18626,#18627);
#15452=AXIS2_PLACEMENT_3D('',#23544,#18628,#18629);
#15453=AXIS2_PLACEMENT_3D('',#23545,#18630,#18631);
#15454=AXIS2_PLACEMENT_3D('',#23546,#18632,#18633);
#15455=AXIS2_PLACEMENT_3D('',#23547,#18634,#18635);
#15456=AXIS2_PLACEMENT_3D('',#23548,#18636,#18637);
#15457=AXIS2_PLACEMENT_3D('',#23549,#18638,#18639);
#15458=AXIS2_PLACEMENT_3D('',#23550,#18640,#18641);
#15459=AXIS2_PLACEMENT_3D('',#23551,#18642,#18643);
#15460=AXIS2_PLACEMENT_3D('',#23552,#18644,#18645);
#15461=AXIS2_PLACEMENT_3D('',#23554,#18646,#18647);
#15462=AXIS2_PLACEMENT_3D('',#23556,#18648,#18649);
#15463=AXIS2_PLACEMENT_3D('',#23557,#18650,#18651);
#15464=AXIS2_PLACEMENT_3D('',#23559,#18652,#18653);
#15465=AXIS2_PLACEMENT_3D('',#23561,#18655,#18656);
#15466=AXIS2_PLACEMENT_3D('',#23563,#18657,#18658);
#15467=AXIS2_PLACEMENT_3D('',#23564,#18659,#18660);
#15468=AXIS2_PLACEMENT_3D('',#23566,#18662,#18663);
#15469=AXIS2_PLACEMENT_3D('',#23568,#18664,#18665);
#15470=AXIS2_PLACEMENT_3D('',#23570,#18666,#18667);
#15471=AXIS2_PLACEMENT_3D('',#23571,#18668,#18669);
#15472=AXIS2_PLACEMENT_3D('',#23573,#18670,#18671);
#15473=AXIS2_PLACEMENT_3D('',#23575,#18673,#18674);
#15474=AXIS2_PLACEMENT_3D('',#23577,#18675,#18676);
#15475=AXIS2_PLACEMENT_3D('',#23578,#18677,#18678);
#15476=AXIS2_PLACEMENT_3D('',#23580,#18680,#18681);
#15477=AXIS2_PLACEMENT_3D('',#23581,#18682,#18683);
#15478=AXIS2_PLACEMENT_3D('',#23582,#18684,#18685);
#15479=AXIS2_PLACEMENT_3D('',#23583,#18686,#18687);
#15480=AXIS2_PLACEMENT_3D('',#23584,#18688,#18689);
#15481=AXIS2_PLACEMENT_3D('',#23585,#18690,#18691);
#15482=AXIS2_PLACEMENT_3D('',#23586,#18692,#18693);
#15483=AXIS2_PLACEMENT_3D('',#23588,#18694,#18695);
#15484=AXIS2_PLACEMENT_3D('',#23589,#18696,#18697);
#15485=AXIS2_PLACEMENT_3D('',#23591,#18698,#18699);
#15486=AXIS2_PLACEMENT_3D('',#23593,#18701,#18702);
#15487=AXIS2_PLACEMENT_3D('',#23595,#18703,#18704);
#15488=AXIS2_PLACEMENT_3D('',#23597,#18706,#18707);
#15489=AXIS2_PLACEMENT_3D('',#23599,#18708,#18709);
#15490=AXIS2_PLACEMENT_3D('',#23601,#18711,#18712);
#15491=AXIS2_PLACEMENT_3D('',#23603,#18713,#18714);
#15492=AXIS2_PLACEMENT_3D('',#23604,#18715,#18716);
#15493=AXIS2_PLACEMENT_3D('',#23606,#18717,#18718);
#15494=AXIS2_PLACEMENT_3D('',#23608,#18720,#18721);
#15495=AXIS2_PLACEMENT_3D('',#23610,#18722,#18723);
#15496=AXIS2_PLACEMENT_3D('',#23612,#18725,#18726);
#15497=AXIS2_PLACEMENT_3D('',#23614,#18727,#18728);
#15498=AXIS2_PLACEMENT_3D('',#23616,#18730,#18731);
#15499=AXIS2_PLACEMENT_3D('',#23617,#18732,#18733);
#15500=AXIS2_PLACEMENT_3D('',#23626,#18738,#18739);
#15501=AXIS2_PLACEMENT_3D('',#23632,#18743,#18744);
#15502=AXIS2_PLACEMENT_3D('',#23638,#18748,#18749);
#15503=AXIS2_PLACEMENT_3D('',#23644,#18753,#18754);
#15504=AXIS2_PLACEMENT_3D('',#23650,#18758,#18759);
#15505=AXIS2_PLACEMENT_3D('',#23653,#18762,#18763);
#15506=AXIS2_PLACEMENT_3D('',#23654,#18764,#18765);
#15507=AXIS2_PLACEMENT_3D('',#23655,#18766,#18767);
#15508=AXIS2_PLACEMENT_3D('',#23656,#18768,#18769);
#15509=AXIS2_PLACEMENT_3D('',#23657,#18770,#18771);
#15510=AXIS2_PLACEMENT_3D('',#23659,#18772,#18773);
#15511=AXIS2_PLACEMENT_3D('',#23662,#18775,#18776);
#15512=AXIS2_PLACEMENT_3D('',#23663,#18777,#18778);
#15513=AXIS2_PLACEMENT_3D('',#23665,#18779,#18780);
#15514=AXIS2_PLACEMENT_3D('',#23668,#18782,#18783);
#15515=AXIS2_PLACEMENT_3D('',#23669,#18784,#18785);
#15516=AXIS2_PLACEMENT_3D('',#23672,#18786,#18787);
#15517=AXIS2_PLACEMENT_3D('',#23673,#18788,#18789);
#15518=AXIS2_PLACEMENT_3D('',#23679,#18792,#18793);
#15519=AXIS2_PLACEMENT_3D('',#23680,#18794,#18795);
#15520=AXIS2_PLACEMENT_3D('',#23685,#18797,#18798);
#15521=AXIS2_PLACEMENT_3D('',#23687,#18800,#18801);
#15522=AXIS2_PLACEMENT_3D('',#23692,#18803,#18804);
#15523=AXIS2_PLACEMENT_3D('',#23694,#18806,#18807);
#15524=AXIS2_PLACEMENT_3D('',#23697,#18810,#18811);
#15525=AXIS2_PLACEMENT_3D('',#23703,#18814,#18815);
#15526=AXIS2_PLACEMENT_3D('',#23704,#18816,#18817);
#15527=AXIS2_PLACEMENT_3D('',#23707,#18820,#18821);
#15528=AXIS2_PLACEMENT_3D('',#23717,#18826,#18827);
#15529=AXIS2_PLACEMENT_3D('',#23719,#18828,#18829);
#15530=AXIS2_PLACEMENT_3D('',#23730,#18836,#18837);
#15531=AXIS2_PLACEMENT_3D('',#23731,#18838,#18839);
#15532=AXIS2_PLACEMENT_3D('',#23732,#18840,#18841);
#15533=AXIS2_PLACEMENT_3D('',#23733,#18842,#18843);
#15534=AXIS2_PLACEMENT_3D('',#23734,#18844,#18845);
#15535=AXIS2_PLACEMENT_3D('',#23735,#18846,#18847);
#15536=AXIS2_PLACEMENT_3D('',#23744,#18852,#18853);
#15537=AXIS2_PLACEMENT_3D('',#23750,#18857,#18858);
#15538=AXIS2_PLACEMENT_3D('',#23756,#18862,#18863);
#15539=AXIS2_PLACEMENT_3D('',#23759,#18866,#18867);
#15540=AXIS2_PLACEMENT_3D('',#23760,#18868,#18869);
#15541=AXIS2_PLACEMENT_3D('',#23762,#18870,#18871);
#15542=AXIS2_PLACEMENT_3D('',#23764,#18873,#18874);
#15543=AXIS2_PLACEMENT_3D('',#23766,#18875,#18876);
#15544=AXIS2_PLACEMENT_3D('',#23768,#18878,#18879);
#15545=AXIS2_PLACEMENT_3D('',#23774,#18883,#18884);
#15546=AXIS2_PLACEMENT_3D('',#23778,#18887,#18888);
#15547=AXIS2_PLACEMENT_3D('',#23782,#18891,#18892);
#15548=AXIS2_PLACEMENT_3D('',#23784,#18894,#18895);
#15549=AXIS2_PLACEMENT_3D('',#23785,#18896,#18897);
#15550=AXIS2_PLACEMENT_3D('',#23786,#18898,#18899);
#15551=AXIS2_PLACEMENT_3D('',#23788,#18900,#18901);
#15552=AXIS2_PLACEMENT_3D('',#23791,#18903,#18904);
#15553=AXIS2_PLACEMENT_3D('',#23792,#18905,#18906);
#15554=AXIS2_PLACEMENT_3D('',#23794,#18907,#18908);
#15555=AXIS2_PLACEMENT_3D('',#23795,#18909,#18910);
#15556=AXIS2_PLACEMENT_3D('',#23798,#18911,#18912);
#15557=AXIS2_PLACEMENT_3D('',#23800,#18913,#18914);
#15558=AXIS2_PLACEMENT_3D('',#23801,#18915,#18916);
#15559=AXIS2_PLACEMENT_3D('',#23802,#18917,#18918);
#15560=AXIS2_PLACEMENT_3D('',#23880,#18920,#18921);
#15561=AXIS2_PLACEMENT_3D('',#23958,#18923,#18924);
#15562=AXIS2_PLACEMENT_3D('',#23960,#18925,#18926);
#15563=AXIS2_PLACEMENT_3D('',#23963,#18928,#18929);
#15564=AXIS2_PLACEMENT_3D('',#24128,#18930,#18931);
#15565=AXIS2_PLACEMENT_3D('',#24165,#18933,#18934);
#15566=AXIS2_PLACEMENT_3D('',#24202,#18936,#18937);
#15567=AXIS2_PLACEMENT_3D('',#24239,#18939,#18940);
#15568=AXIS2_PLACEMENT_3D('',#24276,#18942,#18943);
#15569=AXIS2_PLACEMENT_3D('',#24278,#18944,#18945);
#15570=AXIS2_PLACEMENT_3D('',#24279,#18946,#18947);
#15571=AXIS2_PLACEMENT_3D('',#24281,#18948,#18949);
#15572=AXIS2_PLACEMENT_3D('',#24282,#18950,#18951);
#15573=AXIS2_PLACEMENT_3D('',#24284,#18952,#18953);
#15574=AXIS2_PLACEMENT_3D('',#24286,#18955,#18956);
#15575=AXIS2_PLACEMENT_3D('',#24288,#18957,#18958);
#15576=AXIS2_PLACEMENT_3D('',#24289,#18959,#18960);
#15577=AXIS2_PLACEMENT_3D('',#24291,#18962,#18963);
#15578=AXIS2_PLACEMENT_3D('',#24292,#18964,#18965);
#15579=AXIS2_PLACEMENT_3D('',#24293,#18966,#18967);
#15580=AXIS2_PLACEMENT_3D('',#24294,#18968,#18969);
#15581=AXIS2_PLACEMENT_3D('',#24296,#18970,#18971);
#15582=AXIS2_PLACEMENT_3D('',#24299,#18973,#18974);
#15583=AXIS2_PLACEMENT_3D('',#24300,#18975,#18976);
#15584=AXIS2_PLACEMENT_3D('',#24302,#18977,#18978);
#15585=AXIS2_PLACEMENT_3D('',#24305,#18980,#18981);
#15586=AXIS2_PLACEMENT_3D('',#24306,#18982,#18983);
#15587=AXIS2_PLACEMENT_3D('',#24307,#18984,#18985);
#15588=AXIS2_PLACEMENT_3D('',#24308,#18986,#18987);
#15589=AXIS2_PLACEMENT_3D('',#24309,#18988,#18989);
#15590=AXIS2_PLACEMENT_3D('',#24318,#18994,#18995);
#15591=AXIS2_PLACEMENT_3D('',#24324,#18999,#19000);
#15592=AXIS2_PLACEMENT_3D('',#24330,#19004,#19005);
#15593=AXIS2_PLACEMENT_3D('',#24336,#19009,#19010);
#15594=AXIS2_PLACEMENT_3D('',#24342,#19014,#19015);
#15595=AXIS2_PLACEMENT_3D('',#24345,#19018,#19019);
#15596=AXIS2_PLACEMENT_3D('',#24346,#19020,#19021);
#15597=AXIS2_PLACEMENT_3D('',#24347,#19022,#19023);
#15598=AXIS2_PLACEMENT_3D('',#24349,#19024,#19025);
#15599=AXIS2_PLACEMENT_3D('',#24350,#19026,#19027);
#15600=AXIS2_PLACEMENT_3D('',#24352,#19028,#19029);
#15601=AXIS2_PLACEMENT_3D('',#24353,#19030,#19031);
#15602=AXIS2_PLACEMENT_3D('',#24355,#19032,#19033);
#15603=AXIS2_PLACEMENT_3D('',#24357,#19035,#19036);
#15604=AXIS2_PLACEMENT_3D('',#24359,#19037,#19038);
#15605=AXIS2_PLACEMENT_3D('',#24361,#19040,#19041);
#15606=AXIS2_PLACEMENT_3D('',#24363,#19042,#19043);
#15607=AXIS2_PLACEMENT_3D('',#24365,#19045,#19046);
#15608=AXIS2_PLACEMENT_3D('',#24367,#19047,#19048);
#15609=AXIS2_PLACEMENT_3D('',#24368,#19049,#19050);
#15610=AXIS2_PLACEMENT_3D('',#24370,#19051,#19052);
#15611=AXIS2_PLACEMENT_3D('',#24372,#19054,#19055);
#15612=AXIS2_PLACEMENT_3D('',#24374,#19057,#19058);
#15613=AXIS2_PLACEMENT_3D('',#24375,#19059,#19060);
#15614=AXIS2_PLACEMENT_3D('',#24384,#19065,#19066);
#15615=AXIS2_PLACEMENT_3D('',#24390,#19070,#19071);
#15616=AXIS2_PLACEMENT_3D('',#24396,#19075,#19076);
#15617=AXIS2_PLACEMENT_3D('',#24402,#19080,#19081);
#15618=AXIS2_PLACEMENT_3D('',#24408,#19085,#19086);
#15619=AXIS2_PLACEMENT_3D('',#24411,#19089,#19090);
#15620=AXIS2_PLACEMENT_3D('',#24412,#19091,#19092);
#15621=AXIS2_PLACEMENT_3D('',#24413,#19093,#19094);
#15622=AXIS2_PLACEMENT_3D('',#24415,#19095,#19096);
#15623=AXIS2_PLACEMENT_3D('',#24416,#19097,#19098);
#15624=AXIS2_PLACEMENT_3D('',#24418,#19099,#19100);
#15625=AXIS2_PLACEMENT_3D('',#24419,#19101,#19102);
#15626=AXIS2_PLACEMENT_3D('',#24421,#19103,#19104);
#15627=AXIS2_PLACEMENT_3D('',#24423,#19106,#19107);
#15628=AXIS2_PLACEMENT_3D('',#24425,#19108,#19109);
#15629=AXIS2_PLACEMENT_3D('',#24427,#19111,#19112);
#15630=AXIS2_PLACEMENT_3D('',#24429,#19113,#19114);
#15631=AXIS2_PLACEMENT_3D('',#24431,#19116,#19117);
#15632=AXIS2_PLACEMENT_3D('',#24433,#19118,#19119);
#15633=AXIS2_PLACEMENT_3D('',#24434,#19120,#19121);
#15634=AXIS2_PLACEMENT_3D('',#24436,#19122,#19123);
#15635=AXIS2_PLACEMENT_3D('',#24438,#19125,#19126);
#15636=AXIS2_PLACEMENT_3D('',#24440,#19128,#19129);
#15637=AXIS2_PLACEMENT_3D('',#24441,#19130,#19131);
#15638=AXIS2_PLACEMENT_3D('',#24442,#19132,#19133);
#15639=AXIS2_PLACEMENT_3D('',#24444,#19134,#19135);
#15640=AXIS2_PLACEMENT_3D('',#24447,#19137,#19138);
#15641=AXIS2_PLACEMENT_3D('',#24448,#19139,#19140);
#15642=AXIS2_PLACEMENT_3D('',#24449,#19141,#19142);
#15643=AXIS2_PLACEMENT_3D('',#24451,#19143,#19144);
#15644=AXIS2_PLACEMENT_3D('',#24453,#19145,#19146);
#15645=AXIS2_PLACEMENT_3D('',#24454,#19147,#19148);
#15646=AXIS2_PLACEMENT_3D('',#24456,#19149,#19150);
#15647=AXIS2_PLACEMENT_3D('',#24458,#19151,#19152);
#15648=AXIS2_PLACEMENT_3D('',#24459,#19153,#19154);
#15649=AXIS2_PLACEMENT_3D('',#24461,#19156,#19157);
#15650=AXIS2_PLACEMENT_3D('',#24464,#19159,#19160);
#15651=AXIS2_PLACEMENT_3D('',#24465,#19161,#19162);
#15652=AXIS2_PLACEMENT_3D('',#24467,#19163,#19164);
#15653=AXIS2_PLACEMENT_3D('',#24470,#19166,#19167);
#15654=AXIS2_PLACEMENT_3D('',#24471,#19168,#19169);
#15655=AXIS2_PLACEMENT_3D('',#24472,#19170,#19171);
#15656=AXIS2_PLACEMENT_3D('',#24474,#19172,#19173);
#15657=AXIS2_PLACEMENT_3D('',#24476,#19175,#19176);
#15658=AXIS2_PLACEMENT_3D('',#24477,#19177,#19178);
#15659=AXIS2_PLACEMENT_3D('',#24478,#19179,#19180);
#15660=AXIS2_PLACEMENT_3D('',#24479,#19181,#19182);
#15661=AXIS2_PLACEMENT_3D('',#24481,#19183,#19184);
#15662=AXIS2_PLACEMENT_3D('',#24484,#19186,#19187);
#15663=AXIS2_PLACEMENT_3D('',#24485,#19188,#19189);
#15664=AXIS2_PLACEMENT_3D('',#24487,#19190,#19191);
#15665=AXIS2_PLACEMENT_3D('',#24488,#19192,#19193);
#15666=AXIS2_PLACEMENT_3D('',#24491,#19195,#19196);
#15667=AXIS2_PLACEMENT_3D('',#24492,#19197,#19198);
#15668=AXIS2_PLACEMENT_3D('',#24494,#19199,#19200);
#15669=AXIS2_PLACEMENT_3D('',#24497,#19202,#19203);
#15670=AXIS2_PLACEMENT_3D('',#24498,#19204,#19205);
#15671=AXIS2_PLACEMENT_3D('',#24499,#19206,#19207);
#15672=AXIS2_PLACEMENT_3D('',#24500,#19208,#19209);
#15673=AXIS2_PLACEMENT_3D('',#24501,#19210,#19211);
#15674=AXIS2_PLACEMENT_3D('',#24503,#19212,#19213);
#15675=AXIS2_PLACEMENT_3D('',#24506,#19215,#19216);
#15676=AXIS2_PLACEMENT_3D('',#24507,#19217,#19218);
#15677=AXIS2_PLACEMENT_3D('',#24509,#19219,#19220);
#15678=AXIS2_PLACEMENT_3D('',#24512,#19222,#19223);
#15679=AXIS2_PLACEMENT_3D('',#24513,#19224,#19225);
#15680=AXIS2_PLACEMENT_3D('',#24514,#19226,#19227);
#15681=AXIS2_PLACEMENT_3D('',#24515,#19228,#19229);
#15682=AXIS2_PLACEMENT_3D('',#24516,#19230,#19231);
#15683=AXIS2_PLACEMENT_3D('',#24518,#19232,#19233);
#15684=AXIS2_PLACEMENT_3D('',#24521,#19235,#19236);
#15685=AXIS2_PLACEMENT_3D('',#24522,#19237,#19238);
#15686=AXIS2_PLACEMENT_3D('',#24523,#19239,#19240);
#15687=AXIS2_PLACEMENT_3D('',#24524,#19241,#19242);
#15688=AXIS2_PLACEMENT_3D('',#24525,#19243,#19244);
#15689=AXIS2_PLACEMENT_3D('',#24527,#19245,#19246);
#15690=AXIS2_PLACEMENT_3D('',#24530,#19248,#19249);
#15691=AXIS2_PLACEMENT_3D('',#24531,#19250,#19251);
#15692=AXIS2_PLACEMENT_3D('',#24532,#19252,#19253);
#15693=AXIS2_PLACEMENT_3D('',#24533,#19254,#19255);
#15694=AXIS2_PLACEMENT_3D('',#24534,#19256,#19257);
#15695=AXIS2_PLACEMENT_3D('',#24536,#19258,#19259);
#15696=AXIS2_PLACEMENT_3D('',#24539,#19261,#19262);
#15697=AXIS2_PLACEMENT_3D('',#24540,#19263,#19264);
#15698=AXIS2_PLACEMENT_3D('',#24542,#19265,#19266);
#15699=AXIS2_PLACEMENT_3D('',#24545,#19268,#19269);
#15700=AXIS2_PLACEMENT_3D('',#24546,#19270,#19271);
#15701=AXIS2_PLACEMENT_3D('',#24547,#19272,#19273);
#15702=AXIS2_PLACEMENT_3D('',#24548,#19274,#19275);
#15703=AXIS2_PLACEMENT_3D('',#24549,#19276,#19277);
#15704=AXIS2_PLACEMENT_3D('',#24551,#19278,#19279);
#15705=AXIS2_PLACEMENT_3D('',#24554,#19281,#19282);
#15706=AXIS2_PLACEMENT_3D('',#24555,#19283,#19284);
#15707=AXIS2_PLACEMENT_3D('',#24556,#19285,#19286);
#15708=AXIS2_PLACEMENT_3D('',#24557,#19287,#19288);
#15709=AXIS2_PLACEMENT_3D('',#24558,#19289,#19290);
#15710=AXIS2_PLACEMENT_3D('',#24562,#19292,#19293);
#15711=AXIS2_PLACEMENT_3D('',#24563,#19294,#19295);
#15712=AXIS2_PLACEMENT_3D('',#24576,#19296,#19297);
#15713=AXIS2_PLACEMENT_3D('',#24617,#19299,#19300);
#15714=AXIS2_PLACEMENT_3D('',#24628,#19301,#19302);
#15715=AXIS2_PLACEMENT_3D('',#24630,#19304,#19305);
#15716=AXIS2_PLACEMENT_3D('',#24634,#19307,#19308);
#15717=AXIS2_PLACEMENT_3D('',#24635,#19309,#19310);
#15718=AXIS2_PLACEMENT_3D('',#24648,#19311,#19312);
#15719=AXIS2_PLACEMENT_3D('',#24689,#19314,#19315);
#15720=AXIS2_PLACEMENT_3D('',#24700,#19316,#19317);
#15721=AXIS2_PLACEMENT_3D('',#24702,#19319,#19320);
#15722=AXIS2_PLACEMENT_3D('',#24704,#19321,#19322);
#15723=AXIS2_PLACEMENT_3D('',#24707,#19324,#19325);
#15724=AXIS2_PLACEMENT_3D('',#24708,#19326,#19327);
#15725=AXIS2_PLACEMENT_3D('',#24710,#19328,#19329);
#15726=AXIS2_PLACEMENT_3D('',#24713,#19331,#19332);
#15727=AXIS2_PLACEMENT_3D('',#24714,#19333,#19334);
#15728=AXIS2_PLACEMENT_3D('',#24715,#19335,#19336);
#15729=AXIS2_PLACEMENT_3D('',#24716,#19337,#19338);
#15730=AXIS2_PLACEMENT_3D('',#24717,#19339,#19340);
#15731=AXIS2_PLACEMENT_3D('',#24804,#19342,#19343);
#15732=AXIS2_PLACEMENT_3D('',#24885,#19345,#19346);
#15733=AXIS2_PLACEMENT_3D('',#24887,#19347,#19348);
#15734=AXIS2_PLACEMENT_3D('',#24891,#19351,#19352);
#15735=AXIS2_PLACEMENT_3D('',#24974,#19353,#19354);
#15736=AXIS2_PLACEMENT_3D('',#25014,#19356,#19357);
#15737=AXIS2_PLACEMENT_3D('',#25054,#19359,#19360);
#15738=AXIS2_PLACEMENT_3D('',#25056,#19361,#19362);
#15739=AXIS2_PLACEMENT_3D('',#25060,#19365,#19366);
#15740=AXIS2_PLACEMENT_3D('',#25061,#19367,#19368);
#15741=AXIS2_PLACEMENT_3D('',#25062,#19369,#19370);
#15742=AXIS2_PLACEMENT_3D('',#25064,#19371,#19372);
#15743=AXIS2_PLACEMENT_3D('',#25067,#19373,#19374);
#15744=AXIS2_PLACEMENT_3D('',#25069,#19375,#19376);
#15745=AXIS2_PLACEMENT_3D('',#25071,#19377,#19378);
#15746=AXIS2_PLACEMENT_3D('',#25073,#19379,#19380);
#15747=AXIS2_PLACEMENT_3D('',#25075,#19381,#19382);
#15748=AXIS2_PLACEMENT_3D('',#25077,#19383,#19384);
#15749=AXIS2_PLACEMENT_3D('',#25079,#19385,#19386);
#15750=AXIS2_PLACEMENT_3D('',#25081,#19387,#19388);
#15751=AXIS2_PLACEMENT_3D('',#25083,#19389,#19390);
#15752=AXIS2_PLACEMENT_3D('',#25085,#19391,#19392);
#15753=AXIS2_PLACEMENT_3D('',#25087,#19393,#19394);
#15754=AXIS2_PLACEMENT_3D('',#25089,#19395,#19396);
#15755=AXIS2_PLACEMENT_3D('',#25091,#19397,#19398);
#15756=AXIS2_PLACEMENT_3D('',#25093,#19399,#19400);
#15757=AXIS2_PLACEMENT_3D('',#25095,#19401,#19402);
#15758=AXIS2_PLACEMENT_3D('',#25097,#19403,#19404);
#15759=AXIS2_PLACEMENT_3D('',#25099,#19405,#19406);
#15760=AXIS2_PLACEMENT_3D('',#25101,#19407,#19408);
#15761=AXIS2_PLACEMENT_3D('',#25103,#19409,#19410);
#15762=AXIS2_PLACEMENT_3D('',#25105,#19411,#19412);
#15763=AXIS2_PLACEMENT_3D('',#25107,#19413,#19414);
#15764=AXIS2_PLACEMENT_3D('',#25109,#19415,#19416);
#15765=AXIS2_PLACEMENT_3D('',#25111,#19417,#19418);
#15766=AXIS2_PLACEMENT_3D('',#25113,#19419,#19420);
#15767=AXIS2_PLACEMENT_3D('',#25115,#19421,#19422);
#15768=AXIS2_PLACEMENT_3D('',#25117,#19423,#19424);
#15769=AXIS2_PLACEMENT_3D('',#25119,#19425,#19426);
#15770=AXIS2_PLACEMENT_3D('',#25121,#19427,#19428);
#15771=AXIS2_PLACEMENT_3D('',#25123,#19429,#19430);
#15772=AXIS2_PLACEMENT_3D('',#25125,#19431,#19432);
#15773=AXIS2_PLACEMENT_3D('',#25127,#19433,#19434);
#15774=AXIS2_PLACEMENT_3D('',#25129,#19435,#19436);
#15775=AXIS2_PLACEMENT_3D('',#25131,#19437,#19438);
#15776=AXIS2_PLACEMENT_3D('',#25133,#19439,#19440);
#15777=AXIS2_PLACEMENT_3D('',#25135,#19441,#19442);
#15778=AXIS2_PLACEMENT_3D('',#25137,#19443,#19444);
#15779=AXIS2_PLACEMENT_3D('',#25139,#19445,#19446);
#15780=AXIS2_PLACEMENT_3D('',#25141,#19447,#19448);
#15781=AXIS2_PLACEMENT_3D('',#25143,#19449,#19450);
#15782=AXIS2_PLACEMENT_3D('',#25144,#19451,#19452);
#15783=AXIS2_PLACEMENT_3D('',#25145,#19453,#19454);
#15784=AXIS2_PLACEMENT_3D('',#25147,#19455,#19456);
#15785=AXIS2_PLACEMENT_3D('',#25149,#19458,#19459);
#15786=AXIS2_PLACEMENT_3D('',#25150,#19460,#19461);
#15787=AXIS2_PLACEMENT_3D('',#25152,#19462,#19463);
#15788=AXIS2_PLACEMENT_3D('',#25155,#19464,#19465);
#15789=AXIS2_PLACEMENT_3D('',#25157,#19466,#19467);
#15790=AXIS2_PLACEMENT_3D('',#25159,#19468,#19469);
#15791=AXIS2_PLACEMENT_3D('',#25161,#19470,#19471);
#15792=AXIS2_PLACEMENT_3D('',#25163,#19472,#19473);
#15793=AXIS2_PLACEMENT_3D('',#25165,#19474,#19475);
#15794=AXIS2_PLACEMENT_3D('',#25167,#19476,#19477);
#15795=AXIS2_PLACEMENT_3D('',#25169,#19478,#19479);
#15796=AXIS2_PLACEMENT_3D('',#25171,#19480,#19481);
#15797=AXIS2_PLACEMENT_3D('',#25173,#19482,#19483);
#15798=AXIS2_PLACEMENT_3D('',#25175,#19484,#19485);
#15799=AXIS2_PLACEMENT_3D('',#25177,#19486,#19487);
#15800=AXIS2_PLACEMENT_3D('',#25179,#19488,#19489);
#15801=AXIS2_PLACEMENT_3D('',#25181,#19490,#19491);
#15802=AXIS2_PLACEMENT_3D('',#25183,#19492,#19493);
#15803=AXIS2_PLACEMENT_3D('',#25185,#19494,#19495);
#15804=AXIS2_PLACEMENT_3D('',#25187,#19496,#19497);
#15805=AXIS2_PLACEMENT_3D('',#25189,#19498,#19499);
#15806=AXIS2_PLACEMENT_3D('',#25191,#19500,#19501);
#15807=AXIS2_PLACEMENT_3D('',#25193,#19502,#19503);
#15808=AXIS2_PLACEMENT_3D('',#25195,#19504,#19505);
#15809=AXIS2_PLACEMENT_3D('',#25197,#19506,#19507);
#15810=AXIS2_PLACEMENT_3D('',#25199,#19508,#19509);
#15811=AXIS2_PLACEMENT_3D('',#25201,#19510,#19511);
#15812=AXIS2_PLACEMENT_3D('',#25203,#19512,#19513);
#15813=AXIS2_PLACEMENT_3D('',#25205,#19514,#19515);
#15814=AXIS2_PLACEMENT_3D('',#25207,#19516,#19517);
#15815=AXIS2_PLACEMENT_3D('',#25209,#19518,#19519);
#15816=AXIS2_PLACEMENT_3D('',#25211,#19520,#19521);
#15817=AXIS2_PLACEMENT_3D('',#25213,#19522,#19523);
#15818=AXIS2_PLACEMENT_3D('',#25215,#19524,#19525);
#15819=AXIS2_PLACEMENT_3D('',#25217,#19526,#19527);
#15820=AXIS2_PLACEMENT_3D('',#25219,#19528,#19529);
#15821=AXIS2_PLACEMENT_3D('',#25221,#19530,#19531);
#15822=AXIS2_PLACEMENT_3D('',#25223,#19532,#19533);
#15823=AXIS2_PLACEMENT_3D('',#25225,#19534,#19535);
#15824=AXIS2_PLACEMENT_3D('',#25227,#19536,#19537);
#15825=AXIS2_PLACEMENT_3D('',#25229,#19538,#19539);
#15826=AXIS2_PLACEMENT_3D('',#25231,#19540,#19541);
#15827=AXIS2_PLACEMENT_3D('',#25232,#19542,#19543);
#15828=AXIS2_PLACEMENT_3D('',#25233,#19544,#19545);
#15829=AXIS2_PLACEMENT_3D('',#25235,#19546,#19547);
#15830=AXIS2_PLACEMENT_3D('',#25237,#19549,#19550);
#15831=AXIS2_PLACEMENT_3D('',#25238,#19551,#19552);
#15832=AXIS2_PLACEMENT_3D('',#25241,#19555,#19556);
#15833=AXIS2_PLACEMENT_3D('',#25243,#19558,#19559);
#15834=AXIS2_PLACEMENT_3D('',#25245,#19561,#19562);
#15835=AXIS2_PLACEMENT_3D('',#25247,#19564,#19565);
#15836=AXIS2_PLACEMENT_3D('',#25249,#19567,#19568);
#15837=AXIS2_PLACEMENT_3D('',#25251,#19570,#19571);
#15838=AXIS2_PLACEMENT_3D('',#25253,#19573,#19574);
#15839=AXIS2_PLACEMENT_3D('',#25255,#19576,#19577);
#15840=AXIS2_PLACEMENT_3D('',#25257,#19579,#19580);
#15841=AXIS2_PLACEMENT_3D('',#25259,#19582,#19583);
#15842=AXIS2_PLACEMENT_3D('',#25261,#19585,#19586);
#15843=AXIS2_PLACEMENT_3D('',#25263,#19588,#19589);
#15844=AXIS2_PLACEMENT_3D('',#25265,#19591,#19592);
#15845=AXIS2_PLACEMENT_3D('',#25267,#19594,#19595);
#15846=AXIS2_PLACEMENT_3D('',#25269,#19597,#19598);
#15847=AXIS2_PLACEMENT_3D('',#25271,#19600,#19601);
#15848=AXIS2_PLACEMENT_3D('',#25273,#19603,#19604);
#15849=AXIS2_PLACEMENT_3D('',#25275,#19606,#19607);
#15850=AXIS2_PLACEMENT_3D('',#25277,#19609,#19610);
#15851=AXIS2_PLACEMENT_3D('',#25279,#19612,#19613);
#15852=AXIS2_PLACEMENT_3D('',#25281,#19615,#19616);
#15853=AXIS2_PLACEMENT_3D('',#25283,#19618,#19619);
#15854=AXIS2_PLACEMENT_3D('',#25285,#19621,#19622);
#15855=AXIS2_PLACEMENT_3D('',#25287,#19624,#19625);
#15856=AXIS2_PLACEMENT_3D('',#25289,#19627,#19628);
#15857=AXIS2_PLACEMENT_3D('',#25291,#19630,#19631);
#15858=AXIS2_PLACEMENT_3D('',#25293,#19633,#19634);
#15859=AXIS2_PLACEMENT_3D('',#25295,#19636,#19637);
#15860=AXIS2_PLACEMENT_3D('',#25297,#19639,#19640);
#15861=AXIS2_PLACEMENT_3D('',#25299,#19642,#19643);
#15862=AXIS2_PLACEMENT_3D('',#25301,#19645,#19646);
#15863=AXIS2_PLACEMENT_3D('',#25303,#19648,#19649);
#15864=AXIS2_PLACEMENT_3D('',#25305,#19651,#19652);
#15865=AXIS2_PLACEMENT_3D('',#25307,#19654,#19655);
#15866=AXIS2_PLACEMENT_3D('',#25309,#19657,#19658);
#15867=AXIS2_PLACEMENT_3D('',#25311,#19660,#19661);
#15868=AXIS2_PLACEMENT_3D('',#25313,#19663,#19664);
#15869=AXIS2_PLACEMENT_3D('',#25315,#19666,#19667);
#15870=AXIS2_PLACEMENT_3D('',#25317,#19669,#19670);
#15871=AXIS2_PLACEMENT_3D('',#25318,#19671,#19672);
#15872=AXIS2_PLACEMENT_3D('',#25319,#19673,#19674);
#15873=AXIS2_PLACEMENT_3D('',#25320,#19675,#19676);
#15874=AXIS2_PLACEMENT_3D('',#25322,#19677,#19678);
#15875=AXIS2_PLACEMENT_3D('',#25324,#19679,#19680);
#15876=AXIS2_PLACEMENT_3D('',#25325,#19681,#19682);
#15877=AXIS2_PLACEMENT_3D('',#25327,#19683,#19684);
#15878=AXIS2_PLACEMENT_3D('',#25329,#19686,#19687);
#15879=AXIS2_PLACEMENT_3D('',#25330,#19688,#19689);
#15880=AXIS2_PLACEMENT_3D('',#25332,#19690,#19691);
#15881=AXIS2_PLACEMENT_3D('',#25335,#19693,#19694);
#15882=AXIS2_PLACEMENT_3D('',#25336,#19695,#19696);
#15883=AXIS2_PLACEMENT_3D('',#25337,#19697,#19698);
#15884=AXIS2_PLACEMENT_3D('',#25339,#19699,#19700);
#15885=AXIS2_PLACEMENT_3D('',#25341,#19701,#19702);
#15886=AXIS2_PLACEMENT_3D('',#25342,#19703,#19704);
#15887=AXIS2_PLACEMENT_3D('',#25344,#19706,#19707);
#15888=AXIS2_PLACEMENT_3D('',#25347,#19709,#19710);
#15889=AXIS2_PLACEMENT_3D('',#25348,#19711,#19712);
#15890=AXIS2_PLACEMENT_3D('',#25349,#19713,#19714);
#15891=AXIS2_PLACEMENT_3D('',#25350,#19715,#19716);
#15892=AXIS2_PLACEMENT_3D('',#25352,#19717,#19718);
#15893=AXIS2_PLACEMENT_3D('',#25355,#19720,#19721);
#15894=AXIS2_PLACEMENT_3D('',#25356,#19722,#19723);
#15895=AXIS2_PLACEMENT_3D('',#25358,#19724,#19725);
#15896=AXIS2_PLACEMENT_3D('',#25361,#19727,#19728);
#15897=AXIS2_PLACEMENT_3D('',#25362,#19729,#19730);
#15898=AXIS2_PLACEMENT_3D('',#25363,#19731,#19732);
#15899=AXIS2_PLACEMENT_3D('',#25364,#19733,#19734);
#15900=AXIS2_PLACEMENT_3D('',#25365,#19735,#19736);
#15901=AXIS2_PLACEMENT_3D('',#25367,#19737,#19738);
#15902=AXIS2_PLACEMENT_3D('',#25370,#19740,#19741);
#15903=AXIS2_PLACEMENT_3D('',#25371,#19742,#19743);
#15904=AXIS2_PLACEMENT_3D('',#25373,#19744,#19745);
#15905=AXIS2_PLACEMENT_3D('',#25376,#19747,#19748);
#15906=AXIS2_PLACEMENT_3D('',#25377,#19749,#19750);
#15907=AXIS2_PLACEMENT_3D('',#25378,#19751,#19752);
#15908=AXIS2_PLACEMENT_3D('',#25379,#19753,#19754);
#15909=AXIS2_PLACEMENT_3D('',#25380,#19755,#19756);
#15910=AXIS2_PLACEMENT_3D('',#25382,#19757,#19758);
#15911=AXIS2_PLACEMENT_3D('',#25385,#19760,#19761);
#15912=AXIS2_PLACEMENT_3D('',#25386,#19762,#19763);
#15913=AXIS2_PLACEMENT_3D('',#25387,#19764,#19765);
#15914=AXIS2_PLACEMENT_3D('',#25388,#19766,#19767);
#15915=AXIS2_PLACEMENT_3D('',#25389,#19768,#19769);
#15916=AXIS2_PLACEMENT_3D('',#25391,#19770,#19771);
#15917=AXIS2_PLACEMENT_3D('',#25394,#19773,#19774);
#15918=AXIS2_PLACEMENT_3D('',#25395,#19775,#19776);
#15919=AXIS2_PLACEMENT_3D('',#25396,#19777,#19778);
#15920=AXIS2_PLACEMENT_3D('',#25397,#19779,#19780);
#15921=AXIS2_PLACEMENT_3D('',#25398,#19781,#19782);
#15922=AXIS2_PLACEMENT_3D('',#25400,#19783,#19784);
#15923=AXIS2_PLACEMENT_3D('',#25403,#19786,#19787);
#15924=AXIS2_PLACEMENT_3D('',#25404,#19788,#19789);
#15925=AXIS2_PLACEMENT_3D('',#25406,#19790,#19791);
#15926=AXIS2_PLACEMENT_3D('',#25409,#19793,#19794);
#15927=AXIS2_PLACEMENT_3D('',#25410,#19795,#19796);
#15928=AXIS2_PLACEMENT_3D('',#25411,#19797,#19798);
#15929=AXIS2_PLACEMENT_3D('',#25412,#19799,#19800);
#15930=AXIS2_PLACEMENT_3D('',#25413,#19801,#19802);
#15931=AXIS2_PLACEMENT_3D('',#25417,#19804,#19805);
#15932=AXIS2_PLACEMENT_3D('',#25418,#19806,#19807);
#15933=AXIS2_PLACEMENT_3D('',#25435,#19808,#19809);
#15934=AXIS2_PLACEMENT_3D('',#25476,#19811,#19812);
#15935=AXIS2_PLACEMENT_3D('',#25491,#19813,#19814);
#15936=AXIS2_PLACEMENT_3D('',#25493,#19816,#19817);
#15937=AXIS2_PLACEMENT_3D('',#25495,#19818,#19819);
#15938=AXIS2_PLACEMENT_3D('',#25498,#19821,#19822);
#15939=AXIS2_PLACEMENT_3D('',#25499,#19823,#19824);
#15940=AXIS2_PLACEMENT_3D('',#25501,#19825,#19826);
#15941=AXIS2_PLACEMENT_3D('',#25504,#19828,#19829);
#15942=AXIS2_PLACEMENT_3D('',#25505,#19830,#19831);
#15943=AXIS2_PLACEMENT_3D('',#25506,#19832,#19833);
#15944=AXIS2_PLACEMENT_3D('',#25507,#19834,#19835);
#15945=AXIS2_PLACEMENT_3D('',#25508,#19836,#19837);
#15946=AXIS2_PLACEMENT_3D('',#25512,#19839,#19840);
#15947=AXIS2_PLACEMENT_3D('',#25513,#19841,#19842);
#15948=AXIS2_PLACEMENT_3D('',#25530,#19843,#19844);
#15949=AXIS2_PLACEMENT_3D('',#25571,#19846,#19847);
#15950=AXIS2_PLACEMENT_3D('',#25586,#19848,#19849);
#15951=AXIS2_PLACEMENT_3D('',#25588,#19851,#19852);
#15952=AXIS2_PLACEMENT_3D('',#25590,#19853,#19854);
#15953=AXIS2_PLACEMENT_3D('',#25593,#19856,#19857);
#15954=AXIS2_PLACEMENT_3D('',#25594,#19858,#19859);
#15955=AXIS2_PLACEMENT_3D('',#25596,#19860,#19861);
#15956=AXIS2_PLACEMENT_3D('',#25599,#19863,#19864);
#15957=AXIS2_PLACEMENT_3D('',#25600,#19865,#19866);
#15958=AXIS2_PLACEMENT_3D('',#25601,#19867,#19868);
#15959=AXIS2_PLACEMENT_3D('',#25602,#19869,#19870);
#15960=AXIS2_PLACEMENT_3D('',#25603,#19871,#19872);
#15961=AXIS2_PLACEMENT_3D('',#25605,#19873,#19874);
#15962=AXIS2_PLACEMENT_3D('',#25608,#19876,#19877);
#15963=AXIS2_PLACEMENT_3D('',#25609,#19878,#19879);
#15964=AXIS2_PLACEMENT_3D('',#25611,#19880,#19881);
#15965=AXIS2_PLACEMENT_3D('',#25614,#19883,#19884);
#15966=AXIS2_PLACEMENT_3D('',#25615,#19885,#19886);
#15967=AXIS2_PLACEMENT_3D('',#25616,#19887,#19888);
#15968=AXIS2_PLACEMENT_3D('',#25617,#19889,#19890);
#15969=AXIS2_PLACEMENT_3D('',#25618,#19891,#19892);
#15970=AXIS2_PLACEMENT_3D('',#25620,#19893,#19894);
#15971=AXIS2_PLACEMENT_3D('',#25623,#19896,#19897);
#15972=AXIS2_PLACEMENT_3D('',#25624,#19898,#19899);
#15973=AXIS2_PLACEMENT_3D('',#25626,#19900,#19901);
#15974=AXIS2_PLACEMENT_3D('',#25629,#19903,#19904);
#15975=AXIS2_PLACEMENT_3D('',#25630,#19905,#19906);
#15976=AXIS2_PLACEMENT_3D('',#25631,#19907,#19908);
#15977=AXIS2_PLACEMENT_3D('',#25632,#19909,#19910);
#15978=AXIS2_PLACEMENT_3D('',#25633,#19911,#19912);
#15979=AXIS2_PLACEMENT_3D('',#25635,#19913,#19914);
#15980=AXIS2_PLACEMENT_3D('',#25638,#19916,#19917);
#15981=AXIS2_PLACEMENT_3D('',#25639,#19918,#19919);
#15982=AXIS2_PLACEMENT_3D('',#25641,#19920,#19921);
#15983=AXIS2_PLACEMENT_3D('',#25644,#19923,#19924);
#15984=AXIS2_PLACEMENT_3D('',#25645,#19925,#19926);
#15985=AXIS2_PLACEMENT_3D('',#25646,#19927,#19928);
#15986=AXIS2_PLACEMENT_3D('',#25647,#19929,#19930);
#15987=AXIS2_PLACEMENT_3D('',#25648,#19931,#19932);
#15988=AXIS2_PLACEMENT_3D('',#25652,#19934,#19935);
#15989=AXIS2_PLACEMENT_3D('',#25653,#19936,#19937);
#15990=AXIS2_PLACEMENT_3D('',#25670,#19938,#19939);
#15991=AXIS2_PLACEMENT_3D('',#25711,#19941,#19942);
#15992=AXIS2_PLACEMENT_3D('',#25726,#19943,#19944);
#15993=AXIS2_PLACEMENT_3D('',#25728,#19946,#19947);
#15994=AXIS2_PLACEMENT_3D('',#25730,#19948,#19949);
#15995=AXIS2_PLACEMENT_3D('',#25733,#19951,#19952);
#15996=AXIS2_PLACEMENT_3D('',#25734,#19953,#19954);
#15997=AXIS2_PLACEMENT_3D('',#25736,#19955,#19956);
#15998=AXIS2_PLACEMENT_3D('',#25739,#19958,#19959);
#15999=AXIS2_PLACEMENT_3D('',#25740,#19960,#19961);
#16000=AXIS2_PLACEMENT_3D('',#25741,#19962,#19963);
#16001=AXIS2_PLACEMENT_3D('',#25742,#19964,#19965);
#16002=AXIS2_PLACEMENT_3D('',#25743,#19966,#19967);
#16003=AXIS2_PLACEMENT_3D('',#25747,#19969,#19970);
#16004=AXIS2_PLACEMENT_3D('',#25748,#19971,#19972);
#16005=AXIS2_PLACEMENT_3D('',#25765,#19973,#19974);
#16006=AXIS2_PLACEMENT_3D('',#25806,#19976,#19977);
#16007=AXIS2_PLACEMENT_3D('',#25821,#19978,#19979);
#16008=AXIS2_PLACEMENT_3D('',#25823,#19981,#19982);
#16009=AXIS2_PLACEMENT_3D('',#25825,#19983,#19984);
#16010=AXIS2_PLACEMENT_3D('',#25828,#19986,#19987);
#16011=AXIS2_PLACEMENT_3D('',#25829,#19988,#19989);
#16012=AXIS2_PLACEMENT_3D('',#25831,#19990,#19991);
#16013=AXIS2_PLACEMENT_3D('',#25834,#19993,#19994);
#16014=AXIS2_PLACEMENT_3D('',#25835,#19995,#19996);
#16015=AXIS2_PLACEMENT_3D('',#25836,#19997,#19998);
#16016=AXIS2_PLACEMENT_3D('',#25837,#19999,#20000);
#16017=AXIS2_PLACEMENT_3D('',#25838,#20001,#20002);
#16018=AXIS2_PLACEMENT_3D('',#25925,#20004,#20005);
#16019=AXIS2_PLACEMENT_3D('',#26006,#20007,#20008);
#16020=AXIS2_PLACEMENT_3D('',#26008,#20009,#20010);
#16021=AXIS2_PLACEMENT_3D('',#26012,#20013,#20014);
#16022=AXIS2_PLACEMENT_3D('',#26095,#20015,#20016);
#16023=AXIS2_PLACEMENT_3D('',#26135,#20018,#20019);
#16024=AXIS2_PLACEMENT_3D('',#26175,#20021,#20022);
#16025=AXIS2_PLACEMENT_3D('',#26177,#20023,#20024);
#16026=AXIS2_PLACEMENT_3D('',#26181,#20027,#20028);
#16027=AXIS2_PLACEMENT_3D('',#26182,#20029,#20030);
#16028=AXIS2_PLACEMENT_3D('',#26183,#20031,#20032);
#16029=AXIS2_PLACEMENT_3D('',#26185,#20033,#20034);
#16030=AXIS2_PLACEMENT_3D('',#26188,#20035,#20036);
#16031=AXIS2_PLACEMENT_3D('',#26190,#20037,#20038);
#16032=AXIS2_PLACEMENT_3D('',#26192,#20039,#20040);
#16033=AXIS2_PLACEMENT_3D('',#26194,#20041,#20042);
#16034=AXIS2_PLACEMENT_3D('',#26196,#20043,#20044);
#16035=AXIS2_PLACEMENT_3D('',#26198,#20045,#20046);
#16036=AXIS2_PLACEMENT_3D('',#26200,#20047,#20048);
#16037=AXIS2_PLACEMENT_3D('',#26202,#20049,#20050);
#16038=AXIS2_PLACEMENT_3D('',#26204,#20051,#20052);
#16039=AXIS2_PLACEMENT_3D('',#26206,#20053,#20054);
#16040=AXIS2_PLACEMENT_3D('',#26208,#20055,#20056);
#16041=AXIS2_PLACEMENT_3D('',#26210,#20057,#20058);
#16042=AXIS2_PLACEMENT_3D('',#26212,#20059,#20060);
#16043=AXIS2_PLACEMENT_3D('',#26214,#20061,#20062);
#16044=AXIS2_PLACEMENT_3D('',#26216,#20063,#20064);
#16045=AXIS2_PLACEMENT_3D('',#26218,#20065,#20066);
#16046=AXIS2_PLACEMENT_3D('',#26220,#20067,#20068);
#16047=AXIS2_PLACEMENT_3D('',#26222,#20069,#20070);
#16048=AXIS2_PLACEMENT_3D('',#26224,#20071,#20072);
#16049=AXIS2_PLACEMENT_3D('',#26226,#20073,#20074);
#16050=AXIS2_PLACEMENT_3D('',#26228,#20075,#20076);
#16051=AXIS2_PLACEMENT_3D('',#26230,#20077,#20078);
#16052=AXIS2_PLACEMENT_3D('',#26232,#20079,#20080);
#16053=AXIS2_PLACEMENT_3D('',#26234,#20081,#20082);
#16054=AXIS2_PLACEMENT_3D('',#26236,#20083,#20084);
#16055=AXIS2_PLACEMENT_3D('',#26238,#20085,#20086);
#16056=AXIS2_PLACEMENT_3D('',#26240,#20087,#20088);
#16057=AXIS2_PLACEMENT_3D('',#26242,#20089,#20090);
#16058=AXIS2_PLACEMENT_3D('',#26244,#20091,#20092);
#16059=AXIS2_PLACEMENT_3D('',#26246,#20093,#20094);
#16060=AXIS2_PLACEMENT_3D('',#26248,#20095,#20096);
#16061=AXIS2_PLACEMENT_3D('',#26250,#20097,#20098);
#16062=AXIS2_PLACEMENT_3D('',#26252,#20099,#20100);
#16063=AXIS2_PLACEMENT_3D('',#26254,#20101,#20102);
#16064=AXIS2_PLACEMENT_3D('',#26256,#20103,#20104);
#16065=AXIS2_PLACEMENT_3D('',#26258,#20105,#20106);
#16066=AXIS2_PLACEMENT_3D('',#26260,#20107,#20108);
#16067=AXIS2_PLACEMENT_3D('',#26262,#20109,#20110);
#16068=AXIS2_PLACEMENT_3D('',#26264,#20111,#20112);
#16069=AXIS2_PLACEMENT_3D('',#26266,#20113,#20114);
#16070=AXIS2_PLACEMENT_3D('',#26268,#20115,#20116);
#16071=AXIS2_PLACEMENT_3D('',#26270,#20117,#20118);
#16072=AXIS2_PLACEMENT_3D('',#26272,#20119,#20120);
#16073=AXIS2_PLACEMENT_3D('',#26274,#20121,#20122);
#16074=AXIS2_PLACEMENT_3D('',#26276,#20123,#20124);
#16075=AXIS2_PLACEMENT_3D('',#26278,#20125,#20126);
#16076=AXIS2_PLACEMENT_3D('',#26280,#20127,#20128);
#16077=AXIS2_PLACEMENT_3D('',#26282,#20129,#20130);
#16078=AXIS2_PLACEMENT_3D('',#26284,#20131,#20132);
#16079=AXIS2_PLACEMENT_3D('',#26286,#20133,#20134);
#16080=AXIS2_PLACEMENT_3D('',#26288,#20135,#20136);
#16081=AXIS2_PLACEMENT_3D('',#26290,#20137,#20138);
#16082=AXIS2_PLACEMENT_3D('',#26292,#20139,#20140);
#16083=AXIS2_PLACEMENT_3D('',#26294,#20141,#20142);
#16084=AXIS2_PLACEMENT_3D('',#26296,#20143,#20144);
#16085=AXIS2_PLACEMENT_3D('',#26298,#20145,#20146);
#16086=AXIS2_PLACEMENT_3D('',#26300,#20147,#20148);
#16087=AXIS2_PLACEMENT_3D('',#26302,#20149,#20150);
#16088=AXIS2_PLACEMENT_3D('',#26304,#20151,#20152);
#16089=AXIS2_PLACEMENT_3D('',#26306,#20153,#20154);
#16090=AXIS2_PLACEMENT_3D('',#26308,#20155,#20156);
#16091=AXIS2_PLACEMENT_3D('',#26310,#20157,#20158);
#16092=AXIS2_PLACEMENT_3D('',#26312,#20159,#20160);
#16093=AXIS2_PLACEMENT_3D('',#26314,#20161,#20162);
#16094=AXIS2_PLACEMENT_3D('',#26316,#20163,#20164);
#16095=AXIS2_PLACEMENT_3D('',#26318,#20165,#20166);
#16096=AXIS2_PLACEMENT_3D('',#26320,#20167,#20168);
#16097=AXIS2_PLACEMENT_3D('',#26322,#20169,#20170);
#16098=AXIS2_PLACEMENT_3D('',#26324,#20171,#20172);
#16099=AXIS2_PLACEMENT_3D('',#26326,#20173,#20174);
#16100=AXIS2_PLACEMENT_3D('',#26328,#20175,#20176);
#16101=AXIS2_PLACEMENT_3D('',#26330,#20177,#20178);
#16102=AXIS2_PLACEMENT_3D('',#26332,#20179,#20180);
#16103=AXIS2_PLACEMENT_3D('',#26334,#20181,#20182);
#16104=AXIS2_PLACEMENT_3D('',#26336,#20183,#20184);
#16105=AXIS2_PLACEMENT_3D('',#26338,#20185,#20186);
#16106=AXIS2_PLACEMENT_3D('',#26340,#20187,#20188);
#16107=AXIS2_PLACEMENT_3D('',#26342,#20189,#20190);
#16108=AXIS2_PLACEMENT_3D('',#26344,#20191,#20192);
#16109=AXIS2_PLACEMENT_3D('',#26345,#20193,#20194);
#16110=AXIS2_PLACEMENT_3D('',#26346,#20195,#20196);
#16111=AXIS2_PLACEMENT_3D('',#26348,#20197,#20198);
#16112=AXIS2_PLACEMENT_3D('',#26350,#20200,#20201);
#16113=AXIS2_PLACEMENT_3D('',#26351,#20202,#20203);
#16114=AXIS2_PLACEMENT_3D('',#26353,#20204,#20205);
#16115=AXIS2_PLACEMENT_3D('',#26356,#20206,#20207);
#16116=AXIS2_PLACEMENT_3D('',#26358,#20208,#20209);
#16117=AXIS2_PLACEMENT_3D('',#26360,#20210,#20211);
#16118=AXIS2_PLACEMENT_3D('',#26362,#20212,#20213);
#16119=AXIS2_PLACEMENT_3D('',#26364,#20214,#20215);
#16120=AXIS2_PLACEMENT_3D('',#26366,#20216,#20217);
#16121=AXIS2_PLACEMENT_3D('',#26368,#20218,#20219);
#16122=AXIS2_PLACEMENT_3D('',#26370,#20220,#20221);
#16123=AXIS2_PLACEMENT_3D('',#26372,#20222,#20223);
#16124=AXIS2_PLACEMENT_3D('',#26374,#20224,#20225);
#16125=AXIS2_PLACEMENT_3D('',#26376,#20226,#20227);
#16126=AXIS2_PLACEMENT_3D('',#26378,#20228,#20229);
#16127=AXIS2_PLACEMENT_3D('',#26380,#20230,#20231);
#16128=AXIS2_PLACEMENT_3D('',#26382,#20232,#20233);
#16129=AXIS2_PLACEMENT_3D('',#26384,#20234,#20235);
#16130=AXIS2_PLACEMENT_3D('',#26386,#20236,#20237);
#16131=AXIS2_PLACEMENT_3D('',#26388,#20238,#20239);
#16132=AXIS2_PLACEMENT_3D('',#26390,#20240,#20241);
#16133=AXIS2_PLACEMENT_3D('',#26392,#20242,#20243);
#16134=AXIS2_PLACEMENT_3D('',#26394,#20244,#20245);
#16135=AXIS2_PLACEMENT_3D('',#26396,#20246,#20247);
#16136=AXIS2_PLACEMENT_3D('',#26398,#20248,#20249);
#16137=AXIS2_PLACEMENT_3D('',#26400,#20250,#20251);
#16138=AXIS2_PLACEMENT_3D('',#26402,#20252,#20253);
#16139=AXIS2_PLACEMENT_3D('',#26404,#20254,#20255);
#16140=AXIS2_PLACEMENT_3D('',#26406,#20256,#20257);
#16141=AXIS2_PLACEMENT_3D('',#26408,#20258,#20259);
#16142=AXIS2_PLACEMENT_3D('',#26410,#20260,#20261);
#16143=AXIS2_PLACEMENT_3D('',#26412,#20262,#20263);
#16144=AXIS2_PLACEMENT_3D('',#26414,#20264,#20265);
#16145=AXIS2_PLACEMENT_3D('',#26416,#20266,#20267);
#16146=AXIS2_PLACEMENT_3D('',#26418,#20268,#20269);
#16147=AXIS2_PLACEMENT_3D('',#26420,#20270,#20271);
#16148=AXIS2_PLACEMENT_3D('',#26422,#20272,#20273);
#16149=AXIS2_PLACEMENT_3D('',#26424,#20274,#20275);
#16150=AXIS2_PLACEMENT_3D('',#26426,#20276,#20277);
#16151=AXIS2_PLACEMENT_3D('',#26428,#20278,#20279);
#16152=AXIS2_PLACEMENT_3D('',#26430,#20280,#20281);
#16153=AXIS2_PLACEMENT_3D('',#26432,#20282,#20283);
#16154=AXIS2_PLACEMENT_3D('',#26434,#20284,#20285);
#16155=AXIS2_PLACEMENT_3D('',#26436,#20286,#20287);
#16156=AXIS2_PLACEMENT_3D('',#26438,#20288,#20289);
#16157=AXIS2_PLACEMENT_3D('',#26440,#20290,#20291);
#16158=AXIS2_PLACEMENT_3D('',#26442,#20292,#20293);
#16159=AXIS2_PLACEMENT_3D('',#26444,#20294,#20295);
#16160=AXIS2_PLACEMENT_3D('',#26446,#20296,#20297);
#16161=AXIS2_PLACEMENT_3D('',#26448,#20298,#20299);
#16162=AXIS2_PLACEMENT_3D('',#26450,#20300,#20301);
#16163=AXIS2_PLACEMENT_3D('',#26452,#20302,#20303);
#16164=AXIS2_PLACEMENT_3D('',#26454,#20304,#20305);
#16165=AXIS2_PLACEMENT_3D('',#26456,#20306,#20307);
#16166=AXIS2_PLACEMENT_3D('',#26458,#20308,#20309);
#16167=AXIS2_PLACEMENT_3D('',#26460,#20310,#20311);
#16168=AXIS2_PLACEMENT_3D('',#26462,#20312,#20313);
#16169=AXIS2_PLACEMENT_3D('',#26464,#20314,#20315);
#16170=AXIS2_PLACEMENT_3D('',#26466,#20316,#20317);
#16171=AXIS2_PLACEMENT_3D('',#26468,#20318,#20319);
#16172=AXIS2_PLACEMENT_3D('',#26470,#20320,#20321);
#16173=AXIS2_PLACEMENT_3D('',#26472,#20322,#20323);
#16174=AXIS2_PLACEMENT_3D('',#26474,#20324,#20325);
#16175=AXIS2_PLACEMENT_3D('',#26476,#20326,#20327);
#16176=AXIS2_PLACEMENT_3D('',#26478,#20328,#20329);
#16177=AXIS2_PLACEMENT_3D('',#26480,#20330,#20331);
#16178=AXIS2_PLACEMENT_3D('',#26482,#20332,#20333);
#16179=AXIS2_PLACEMENT_3D('',#26484,#20334,#20335);
#16180=AXIS2_PLACEMENT_3D('',#26486,#20336,#20337);
#16181=AXIS2_PLACEMENT_3D('',#26488,#20338,#20339);
#16182=AXIS2_PLACEMENT_3D('',#26490,#20340,#20341);
#16183=AXIS2_PLACEMENT_3D('',#26492,#20342,#20343);
#16184=AXIS2_PLACEMENT_3D('',#26494,#20344,#20345);
#16185=AXIS2_PLACEMENT_3D('',#26496,#20346,#20347);
#16186=AXIS2_PLACEMENT_3D('',#26498,#20348,#20349);
#16187=AXIS2_PLACEMENT_3D('',#26500,#20350,#20351);
#16188=AXIS2_PLACEMENT_3D('',#26502,#20352,#20353);
#16189=AXIS2_PLACEMENT_3D('',#26504,#20354,#20355);
#16190=AXIS2_PLACEMENT_3D('',#26506,#20356,#20357);
#16191=AXIS2_PLACEMENT_3D('',#26508,#20358,#20359);
#16192=AXIS2_PLACEMENT_3D('',#26510,#20360,#20361);
#16193=AXIS2_PLACEMENT_3D('',#26512,#20362,#20363);
#16194=AXIS2_PLACEMENT_3D('',#26513,#20364,#20365);
#16195=AXIS2_PLACEMENT_3D('',#26514,#20366,#20367);
#16196=AXIS2_PLACEMENT_3D('',#26516,#20368,#20369);
#16197=AXIS2_PLACEMENT_3D('',#26518,#20371,#20372);
#16198=AXIS2_PLACEMENT_3D('',#26519,#20373,#20374);
#16199=AXIS2_PLACEMENT_3D('',#26522,#20377,#20378);
#16200=AXIS2_PLACEMENT_3D('',#26524,#20380,#20381);
#16201=AXIS2_PLACEMENT_3D('',#26526,#20383,#20384);
#16202=AXIS2_PLACEMENT_3D('',#26528,#20386,#20387);
#16203=AXIS2_PLACEMENT_3D('',#26530,#20389,#20390);
#16204=AXIS2_PLACEMENT_3D('',#26532,#20392,#20393);
#16205=AXIS2_PLACEMENT_3D('',#26534,#20395,#20396);
#16206=AXIS2_PLACEMENT_3D('',#26536,#20398,#20399);
#16207=AXIS2_PLACEMENT_3D('',#26538,#20401,#20402);
#16208=AXIS2_PLACEMENT_3D('',#26540,#20404,#20405);
#16209=AXIS2_PLACEMENT_3D('',#26542,#20407,#20408);
#16210=AXIS2_PLACEMENT_3D('',#26544,#20410,#20411);
#16211=AXIS2_PLACEMENT_3D('',#26546,#20413,#20414);
#16212=AXIS2_PLACEMENT_3D('',#26548,#20416,#20417);
#16213=AXIS2_PLACEMENT_3D('',#26550,#20419,#20420);
#16214=AXIS2_PLACEMENT_3D('',#26552,#20422,#20423);
#16215=AXIS2_PLACEMENT_3D('',#26554,#20425,#20426);
#16216=AXIS2_PLACEMENT_3D('',#26556,#20428,#20429);
#16217=AXIS2_PLACEMENT_3D('',#26558,#20431,#20432);
#16218=AXIS2_PLACEMENT_3D('',#26560,#20434,#20435);
#16219=AXIS2_PLACEMENT_3D('',#26562,#20437,#20438);
#16220=AXIS2_PLACEMENT_3D('',#26564,#20440,#20441);
#16221=AXIS2_PLACEMENT_3D('',#26566,#20443,#20444);
#16222=AXIS2_PLACEMENT_3D('',#26568,#20446,#20447);
#16223=AXIS2_PLACEMENT_3D('',#26570,#20449,#20450);
#16224=AXIS2_PLACEMENT_3D('',#26572,#20452,#20453);
#16225=AXIS2_PLACEMENT_3D('',#26574,#20455,#20456);
#16226=AXIS2_PLACEMENT_3D('',#26576,#20458,#20459);
#16227=AXIS2_PLACEMENT_3D('',#26578,#20461,#20462);
#16228=AXIS2_PLACEMENT_3D('',#26580,#20464,#20465);
#16229=AXIS2_PLACEMENT_3D('',#26582,#20467,#20468);
#16230=AXIS2_PLACEMENT_3D('',#26584,#20470,#20471);
#16231=AXIS2_PLACEMENT_3D('',#26586,#20473,#20474);
#16232=AXIS2_PLACEMENT_3D('',#26588,#20476,#20477);
#16233=AXIS2_PLACEMENT_3D('',#26590,#20479,#20480);
#16234=AXIS2_PLACEMENT_3D('',#26592,#20482,#20483);
#16235=AXIS2_PLACEMENT_3D('',#26594,#20485,#20486);
#16236=AXIS2_PLACEMENT_3D('',#26596,#20488,#20489);
#16237=AXIS2_PLACEMENT_3D('',#26598,#20491,#20492);
#16238=AXIS2_PLACEMENT_3D('',#26600,#20494,#20495);
#16239=AXIS2_PLACEMENT_3D('',#26602,#20497,#20498);
#16240=AXIS2_PLACEMENT_3D('',#26604,#20500,#20501);
#16241=AXIS2_PLACEMENT_3D('',#26606,#20503,#20504);
#16242=AXIS2_PLACEMENT_3D('',#26608,#20506,#20507);
#16243=AXIS2_PLACEMENT_3D('',#26610,#20509,#20510);
#16244=AXIS2_PLACEMENT_3D('',#26612,#20512,#20513);
#16245=AXIS2_PLACEMENT_3D('',#26614,#20515,#20516);
#16246=AXIS2_PLACEMENT_3D('',#26616,#20518,#20519);
#16247=AXIS2_PLACEMENT_3D('',#26618,#20521,#20522);
#16248=AXIS2_PLACEMENT_3D('',#26620,#20524,#20525);
#16249=AXIS2_PLACEMENT_3D('',#26622,#20527,#20528);
#16250=AXIS2_PLACEMENT_3D('',#26624,#20530,#20531);
#16251=AXIS2_PLACEMENT_3D('',#26626,#20533,#20534);
#16252=AXIS2_PLACEMENT_3D('',#26628,#20536,#20537);
#16253=AXIS2_PLACEMENT_3D('',#26630,#20539,#20540);
#16254=AXIS2_PLACEMENT_3D('',#26632,#20542,#20543);
#16255=AXIS2_PLACEMENT_3D('',#26634,#20545,#20546);
#16256=AXIS2_PLACEMENT_3D('',#26636,#20548,#20549);
#16257=AXIS2_PLACEMENT_3D('',#26638,#20551,#20552);
#16258=AXIS2_PLACEMENT_3D('',#26640,#20554,#20555);
#16259=AXIS2_PLACEMENT_3D('',#26642,#20557,#20558);
#16260=AXIS2_PLACEMENT_3D('',#26644,#20560,#20561);
#16261=AXIS2_PLACEMENT_3D('',#26646,#20563,#20564);
#16262=AXIS2_PLACEMENT_3D('',#26648,#20566,#20567);
#16263=AXIS2_PLACEMENT_3D('',#26650,#20569,#20570);
#16264=AXIS2_PLACEMENT_3D('',#26652,#20572,#20573);
#16265=AXIS2_PLACEMENT_3D('',#26654,#20575,#20576);
#16266=AXIS2_PLACEMENT_3D('',#26656,#20578,#20579);
#16267=AXIS2_PLACEMENT_3D('',#26658,#20581,#20582);
#16268=AXIS2_PLACEMENT_3D('',#26660,#20584,#20585);
#16269=AXIS2_PLACEMENT_3D('',#26662,#20587,#20588);
#16270=AXIS2_PLACEMENT_3D('',#26664,#20590,#20591);
#16271=AXIS2_PLACEMENT_3D('',#26666,#20593,#20594);
#16272=AXIS2_PLACEMENT_3D('',#26668,#20596,#20597);
#16273=AXIS2_PLACEMENT_3D('',#26670,#20599,#20600);
#16274=AXIS2_PLACEMENT_3D('',#26672,#20602,#20603);
#16275=AXIS2_PLACEMENT_3D('',#26674,#20605,#20606);
#16276=AXIS2_PLACEMENT_3D('',#26676,#20608,#20609);
#16277=AXIS2_PLACEMENT_3D('',#26678,#20611,#20612);
#16278=AXIS2_PLACEMENT_3D('',#26679,#20613,#20614);
#16279=AXIS2_PLACEMENT_3D('',#26680,#20615,#20616);
#16280=AXIS2_PLACEMENT_3D('',#26682,#20617,#20618);
#16281=AXIS2_PLACEMENT_3D('',#26683,#20619,#20620);
#16282=AXIS2_PLACEMENT_3D('',#26685,#20621,#20622);
#16283=AXIS2_PLACEMENT_3D('',#26687,#20624,#20625);
#16284=AXIS2_PLACEMENT_3D('',#26689,#20626,#20627);
#16285=AXIS2_PLACEMENT_3D('',#26691,#20629,#20630);
#16286=AXIS2_PLACEMENT_3D('',#26693,#20631,#20632);
#16287=AXIS2_PLACEMENT_3D('',#26695,#20634,#20635);
#16288=AXIS2_PLACEMENT_3D('',#26697,#20636,#20637);
#16289=AXIS2_PLACEMENT_3D('',#26698,#20638,#20639);
#16290=AXIS2_PLACEMENT_3D('',#26700,#20640,#20641);
#16291=AXIS2_PLACEMENT_3D('',#26702,#20643,#20644);
#16292=AXIS2_PLACEMENT_3D('',#26704,#20645,#20646);
#16293=AXIS2_PLACEMENT_3D('',#26706,#20648,#20649);
#16294=AXIS2_PLACEMENT_3D('',#26708,#20650,#20651);
#16295=AXIS2_PLACEMENT_3D('',#26710,#20653,#20654);
#16296=AXIS2_PLACEMENT_3D('',#26711,#20655,#20656);
#16297=AXIS2_PLACEMENT_3D('',#26720,#20661,#20662);
#16298=AXIS2_PLACEMENT_3D('',#26726,#20666,#20667);
#16299=AXIS2_PLACEMENT_3D('',#26732,#20671,#20672);
#16300=AXIS2_PLACEMENT_3D('',#26738,#20676,#20677);
#16301=AXIS2_PLACEMENT_3D('',#26744,#20681,#20682);
#16302=AXIS2_PLACEMENT_3D('',#26747,#20685,#20686);
#16303=AXIS2_PLACEMENT_3D('',#26748,#20687,#20688);
#16304=AXIS2_PLACEMENT_3D('',#26749,#20689,#20690);
#16305=AXIS2_PLACEMENT_3D('',#26750,#20691,#20692);
#16306=AXIS2_PLACEMENT_3D('',#26751,#20693,#20694);
#16307=AXIS2_PLACEMENT_3D('',#26752,#20695,#20696);
#16308=AXIS2_PLACEMENT_3D('',#26753,#20697,#20698);
#16309=AXIS2_PLACEMENT_3D('',#26754,#20699,#20700);
#16310=AXIS2_PLACEMENT_3D('',#26755,#20701,#20702);
#16311=AXIS2_PLACEMENT_3D('',#26756,#20703,#20704);
#16312=AXIS2_PLACEMENT_3D('',#26757,#20705,#20706);
#16313=AXIS2_PLACEMENT_3D('',#26758,#20707,#20708);
#16314=AXIS2_PLACEMENT_3D('',#26759,#20709,#20710);
#16315=AXIS2_PLACEMENT_3D('',#26760,#20711,#20712);
#16316=AXIS2_PLACEMENT_3D('',#26761,#20713,#20714);
#16317=AXIS2_PLACEMENT_3D('',#26762,#20715,#20716);
#16318=AXIS2_PLACEMENT_3D('',#26763,#20717,#20718);
#16319=AXIS2_PLACEMENT_3D('',#26764,#20719,#20720);
#16320=AXIS2_PLACEMENT_3D('',#26765,#20721,#20722);
#16321=AXIS2_PLACEMENT_3D('',#26766,#20723,#20724);
#16322=AXIS2_PLACEMENT_3D('',#26767,#20725,#20726);
#16323=AXIS2_PLACEMENT_3D('',#26768,#20727,#20728);
#16324=AXIS2_PLACEMENT_3D('',#26769,#20729,#20730);
#16325=AXIS2_PLACEMENT_3D('',#26770,#20731,#20732);
#16326=AXIS2_PLACEMENT_3D('',#26771,#20733,#20734);
#16327=AXIS2_PLACEMENT_3D('',#26772,#20735,#20736);
#16328=AXIS2_PLACEMENT_3D('',#26773,#20737,#20738);
#16329=AXIS2_PLACEMENT_3D('',#26774,#20739,#20740);
#16330=AXIS2_PLACEMENT_3D('',#26775,#20741,#20742);
#16331=AXIS2_PLACEMENT_3D('',#26776,#20743,#20744);
#16332=AXIS2_PLACEMENT_3D('',#26777,#20745,#20746);
#16333=AXIS2_PLACEMENT_3D('',#26778,#20747,#20748);
#16334=AXIS2_PLACEMENT_3D('',#26779,#20749,#20750);
#16335=AXIS2_PLACEMENT_3D('',#26780,#20751,#20752);
#16336=AXIS2_PLACEMENT_3D('',#26781,#20753,#20754);
#16337=AXIS2_PLACEMENT_3D('',#26782,#20755,#20756);
#16338=AXIS2_PLACEMENT_3D('',#26783,#20757,#20758);
#16339=AXIS2_PLACEMENT_3D('',#26784,#20759,#20760);
#16340=AXIS2_PLACEMENT_3D('',#26785,#20761,#20762);
#16341=AXIS2_PLACEMENT_3D('',#26786,#20763,#20764);
#16342=AXIS2_PLACEMENT_3D('',#26787,#20765,#20766);
#16343=AXIS2_PLACEMENT_3D('',#26788,#20767,#20768);
#16344=AXIS2_PLACEMENT_3D('',#26789,#20769,#20770);
#16345=AXIS2_PLACEMENT_3D('',#26790,#20771,#20772);
#16346=AXIS2_PLACEMENT_3D('',#26791,#20773,#20774);
#16347=AXIS2_PLACEMENT_3D('',#26792,#20775,#20776);
#16348=AXIS2_PLACEMENT_3D('',#26793,#20777,#20778);
#16349=AXIS2_PLACEMENT_3D('',#26794,#20779,#20780);
#16350=AXIS2_PLACEMENT_3D('',#26795,#20781,#20782);
#16351=AXIS2_PLACEMENT_3D('',#26796,#20783,#20784);
#16352=AXIS2_PLACEMENT_3D('',#26797,#20785,#20786);
#16353=AXIS2_PLACEMENT_3D('',#26798,#20787,#20788);
#16354=AXIS2_PLACEMENT_3D('',#26799,#20789,#20790);
#16355=AXIS2_PLACEMENT_3D('',#26800,#20791,#20792);
#16356=AXIS2_PLACEMENT_3D('',#26801,#20793,#20794);
#16357=AXIS2_PLACEMENT_3D('',#26802,#20795,#20796);
#16358=AXIS2_PLACEMENT_3D('',#26803,#20797,#20798);
#16359=AXIS2_PLACEMENT_3D('',#26804,#20799,#20800);
#16360=AXIS2_PLACEMENT_3D('',#26805,#20801,#20802);
#16361=AXIS2_PLACEMENT_3D('',#26806,#20803,#20804);
#16362=AXIS2_PLACEMENT_3D('',#26807,#20805,#20806);
#16363=AXIS2_PLACEMENT_3D('',#26808,#20807,#20808);
#16364=AXIS2_PLACEMENT_3D('',#26809,#20809,#20810);
#16365=AXIS2_PLACEMENT_3D('',#26810,#20811,#20812);
#16366=AXIS2_PLACEMENT_3D('',#26811,#20813,#20814);
#16367=AXIS2_PLACEMENT_3D('',#26812,#20815,#20816);
#16368=AXIS2_PLACEMENT_3D('',#26813,#20817,#20818);
#16369=AXIS2_PLACEMENT_3D('',#26814,#20819,#20820);
#16370=AXIS2_PLACEMENT_3D('',#26815,#20821,#20822);
#16371=AXIS2_PLACEMENT_3D('',#26816,#20823,#20824);
#16372=AXIS2_PLACEMENT_3D('',#26817,#20825,#20826);
#16373=AXIS2_PLACEMENT_3D('',#26818,#20827,#20828);
#16374=AXIS2_PLACEMENT_3D('',#26819,#20829,#20830);
#16375=AXIS2_PLACEMENT_3D('',#26820,#20831,#20832);
#16376=AXIS2_PLACEMENT_3D('',#26821,#20833,#20834);
#16377=AXIS2_PLACEMENT_3D('',#26822,#20835,#20836);
#16378=AXIS2_PLACEMENT_3D('',#26823,#20837,#20838);
#16379=AXIS2_PLACEMENT_3D('',#26824,#20839,#20840);
#16380=AXIS2_PLACEMENT_3D('',#26825,#20841,#20842);
#16381=AXIS2_PLACEMENT_3D('',#26826,#20843,#20844);
#16382=AXIS2_PLACEMENT_3D('',#26827,#20845,#20846);
#16383=AXIS2_PLACEMENT_3D('',#26828,#20847,#20848);
#16384=AXIS2_PLACEMENT_3D('',#26829,#20849,#20850);
#16385=AXIS2_PLACEMENT_3D('',#26838,#20855,#20856);
#16386=AXIS2_PLACEMENT_3D('',#26844,#20860,#20861);
#16387=AXIS2_PLACEMENT_3D('',#26850,#20865,#20866);
#16388=AXIS2_PLACEMENT_3D('',#26856,#20870,#20871);
#16389=AXIS2_PLACEMENT_3D('',#26862,#20875,#20876);
#16390=AXIS2_PLACEMENT_3D('',#26865,#20879,#20880);
#16391=AXIS2_PLACEMENT_3D('',#26866,#20881,#20882);
#16392=AXIS2_PLACEMENT_3D('',#26868,#20883,#20884);
#16393=AXIS2_PLACEMENT_3D('',#26869,#20885,#20886);
#16394=AXIS2_PLACEMENT_3D('',#26871,#20887,#20888);
#16395=AXIS2_PLACEMENT_3D('',#26873,#20890,#20891);
#16396=AXIS2_PLACEMENT_3D('',#26875,#20892,#20893);
#16397=AXIS2_PLACEMENT_3D('',#26877,#20895,#20896);
#16398=AXIS2_PLACEMENT_3D('',#26879,#20897,#20898);
#16399=AXIS2_PLACEMENT_3D('',#26881,#20900,#20901);
#16400=AXIS2_PLACEMENT_3D('',#26882,#20902,#20903);
#16401=AXIS2_PLACEMENT_3D('',#26883,#20904,#20905);
#16402=AXIS2_PLACEMENT_3D('',#26884,#20906,#20907);
#16403=AXIS2_PLACEMENT_3D('',#26885,#20908,#20909);
#16404=AXIS2_PLACEMENT_3D('',#26886,#20910,#20911);
#16405=AXIS2_PLACEMENT_3D('',#26887,#20912,#20913);
#16406=AXIS2_PLACEMENT_3D('',#26888,#20914,#20915);
#16407=AXIS2_PLACEMENT_3D('',#26889,#20916,#20917);
#16408=AXIS2_PLACEMENT_3D('',#26890,#20918,#20919);
#16409=AXIS2_PLACEMENT_3D('',#26891,#20920,#20921);
#16410=AXIS2_PLACEMENT_3D('',#26892,#20922,#20923);
#16411=AXIS2_PLACEMENT_3D('',#26893,#20924,#20925);
#16412=AXIS2_PLACEMENT_3D('',#26894,#20926,#20927);
#16413=AXIS2_PLACEMENT_3D('',#26895,#20928,#20929);
#16414=AXIS2_PLACEMENT_3D('',#26896,#20930,#20931);
#16415=AXIS2_PLACEMENT_3D('',#26897,#20932,#20933);
#16416=AXIS2_PLACEMENT_3D('',#26898,#20934,#20935);
#16417=AXIS2_PLACEMENT_3D('',#26899,#20936,#20937);
#16418=AXIS2_PLACEMENT_3D('',#26900,#20938,#20939);
#16419=AXIS2_PLACEMENT_3D('',#26901,#20940,#20941);
#16420=AXIS2_PLACEMENT_3D('',#26902,#20942,#20943);
#16421=AXIS2_PLACEMENT_3D('',#26903,#20944,#20945);
#16422=AXIS2_PLACEMENT_3D('',#26904,#20946,#20947);
#16423=AXIS2_PLACEMENT_3D('',#26905,#20948,#20949);
#16424=AXIS2_PLACEMENT_3D('',#26906,#20950,#20951);
#16425=AXIS2_PLACEMENT_3D('',#26907,#20952,#20953);
#16426=AXIS2_PLACEMENT_3D('',#26908,#20954,#20955);
#16427=AXIS2_PLACEMENT_3D('',#26909,#20956,#20957);
#16428=AXIS2_PLACEMENT_3D('',#26910,#20958,#20959);
#16429=AXIS2_PLACEMENT_3D('',#26911,#20960,#20961);
#16430=AXIS2_PLACEMENT_3D('',#26912,#20962,#20963);
#16431=AXIS2_PLACEMENT_3D('',#26913,#20964,#20965);
#16432=AXIS2_PLACEMENT_3D('',#26914,#20966,#20967);
#16433=AXIS2_PLACEMENT_3D('',#26915,#20968,#20969);
#16434=DIRECTION('axis',(0.,0.,1.));
#16435=DIRECTION('refdir',(1.,0.,0.));
#16436=DIRECTION('axis',(0.,0.,1.));
#16437=DIRECTION('refdir',(1.,0.,0.));
#16438=DIRECTION('axis',(0.,0.,1.));
#16439=DIRECTION('refdir',(1.,0.,0.));
#16440=DIRECTION('center_axis',(0.,0.,1.));
#16441=DIRECTION('ref_axis',(1.,0.,0.));
#16442=DIRECTION('center_axis',(0.,0.,1.));
#16443=DIRECTION('ref_axis',(1.,0.,0.));
#16444=DIRECTION('',(0.,0.,1.));
#16445=DIRECTION('center_axis',(0.,0.,-1.));
#16446=DIRECTION('ref_axis',(1.,0.,0.));
#16447=DIRECTION('center_axis',(0.,0.,1.));
#16448=DIRECTION('ref_axis',(1.,0.,0.));
#16449=DIRECTION('center_axis',(0.,0.,1.));
#16450=DIRECTION('ref_axis',(1.,0.,0.));
#16451=DIRECTION('center_axis',(0.,0.,1.));
#16452=DIRECTION('ref_axis',(1.,0.,0.));
#16453=DIRECTION('',(0.,0.,1.));
#16454=DIRECTION('center_axis',(0.,0.,-1.));
#16455=DIRECTION('ref_axis',(1.,0.,0.));
#16456=DIRECTION('center_axis',(0.,0.,1.));
#16457=DIRECTION('ref_axis',(1.,0.,0.));
#16458=DIRECTION('center_axis',(0.,0.,1.));
#16459=DIRECTION('ref_axis',(1.,0.,0.));
#16460=DIRECTION('center_axis',(0.,0.,1.));
#16461=DIRECTION('ref_axis',(1.,0.,0.));
#16462=DIRECTION('',(0.,0.,1.));
#16463=DIRECTION('center_axis',(0.,0.,-1.));
#16464=DIRECTION('ref_axis',(1.,0.,0.));
#16465=DIRECTION('center_axis',(0.,0.,1.));
#16466=DIRECTION('ref_axis',(1.,0.,0.));
#16467=DIRECTION('center_axis',(0.,0.,1.));
#16468=DIRECTION('ref_axis',(1.,0.,0.));
#16469=DIRECTION('center_axis',(0.,0.,1.));
#16470=DIRECTION('ref_axis',(1.,0.,0.));
#16471=DIRECTION('',(0.,0.,1.));
#16472=DIRECTION('center_axis',(0.,0.,-1.));
#16473=DIRECTION('ref_axis',(1.,0.,0.));
#16474=DIRECTION('center_axis',(0.,0.,1.));
#16475=DIRECTION('ref_axis',(1.,0.,0.));
#16476=DIRECTION('center_axis',(0.,0.,1.));
#16477=DIRECTION('ref_axis',(1.,0.,0.));
#16478=DIRECTION('center_axis',(0.,0.,1.));
#16479=DIRECTION('ref_axis',(1.,0.,0.));
#16480=DIRECTION('',(0.,0.,1.));
#16481=DIRECTION('center_axis',(0.,0.,-1.));
#16482=DIRECTION('ref_axis',(1.,0.,0.));
#16483=DIRECTION('center_axis',(0.,0.,1.));
#16484=DIRECTION('ref_axis',(1.,0.,0.));
#16485=DIRECTION('center_axis',(0.,0.,1.));
#16486=DIRECTION('ref_axis',(1.,0.,0.));
#16487=DIRECTION('center_axis',(0.,0.,1.));
#16488=DIRECTION('ref_axis',(1.,0.,0.));
#16489=DIRECTION('',(0.,0.,1.));
#16490=DIRECTION('center_axis',(0.,0.,-1.));
#16491=DIRECTION('ref_axis',(1.,0.,0.));
#16492=DIRECTION('center_axis',(0.,0.,1.));
#16493=DIRECTION('ref_axis',(1.,0.,0.));
#16494=DIRECTION('center_axis',(0.,0.,1.));
#16495=DIRECTION('ref_axis',(1.,0.,0.));
#16496=DIRECTION('center_axis',(0.,0.,1.));
#16497=DIRECTION('ref_axis',(1.,0.,0.));
#16498=DIRECTION('',(0.,0.,1.));
#16499=DIRECTION('center_axis',(0.,0.,-1.));
#16500=DIRECTION('ref_axis',(1.,0.,0.));
#16501=DIRECTION('center_axis',(0.,0.,1.));
#16502=DIRECTION('ref_axis',(1.,0.,0.));
#16503=DIRECTION('center_axis',(0.,0.,1.));
#16504=DIRECTION('ref_axis',(1.,0.,0.));
#16505=DIRECTION('center_axis',(0.,0.,1.));
#16506=DIRECTION('ref_axis',(1.,0.,0.));
#16507=DIRECTION('',(0.,0.,1.));
#16508=DIRECTION('center_axis',(0.,0.,-1.));
#16509=DIRECTION('ref_axis',(1.,0.,0.));
#16510=DIRECTION('center_axis',(0.,0.,1.));
#16511=DIRECTION('ref_axis',(1.,0.,0.));
#16512=DIRECTION('center_axis',(0.,0.,1.));
#16513=DIRECTION('ref_axis',(1.,0.,0.));
#16514=DIRECTION('center_axis',(0.,0.,1.));
#16515=DIRECTION('ref_axis',(1.,0.,0.));
#16516=DIRECTION('',(0.,0.,1.));
#16517=DIRECTION('center_axis',(0.,0.,-1.));
#16518=DIRECTION('ref_axis',(1.,0.,0.));
#16519=DIRECTION('center_axis',(0.,0.,1.));
#16520=DIRECTION('ref_axis',(1.,0.,0.));
#16521=DIRECTION('center_axis',(0.,0.,1.));
#16522=DIRECTION('ref_axis',(1.,0.,0.));
#16523=DIRECTION('center_axis',(0.,0.,1.));
#16524=DIRECTION('ref_axis',(1.,0.,0.));
#16525=DIRECTION('',(0.,0.,1.));
#16526=DIRECTION('center_axis',(0.,0.,-1.));
#16527=DIRECTION('ref_axis',(1.,0.,0.));
#16528=DIRECTION('center_axis',(0.,0.,1.));
#16529=DIRECTION('ref_axis',(1.,0.,0.));
#16530=DIRECTION('center_axis',(0.,0.,1.));
#16531=DIRECTION('ref_axis',(-1.,-1.22464679914735E-16,0.));
#16532=DIRECTION('',(0.,0.,1.));
#16533=DIRECTION('center_axis',(0.,0.,1.));
#16534=DIRECTION('ref_axis',(1.,0.,0.));
#16535=DIRECTION('',(0.,0.,1.));
#16536=DIRECTION('center_axis',(0.,0.,-1.));
#16537=DIRECTION('ref_axis',(1.,0.,0.));
#16538=DIRECTION('center_axis',(0.,0.,1.));
#16539=DIRECTION('ref_axis',(1.,0.,0.));
#16540=DIRECTION('',(0.,0.,1.));
#16541=DIRECTION('center_axis',(0.,0.,-1.));
#16542=DIRECTION('ref_axis',(1.,0.,0.));
#16543=DIRECTION('',(0.,0.,1.));
#16544=DIRECTION('center_axis',(0.,0.,1.));
#16545=DIRECTION('ref_axis',(1.,0.,0.));
#16546=DIRECTION('center_axis',(0.,0.,1.));
#16547=DIRECTION('ref_axis',(1.,0.,0.));
#16548=DIRECTION('',(0.,-1.,0.));
#16549=DIRECTION('',(-1.,0.,0.));
#16550=DIRECTION('',(0.,1.,0.));
#16551=DIRECTION('',(1.,0.,0.));
#16552=DIRECTION('center_axis',(0.,0.,1.));
#16553=DIRECTION('ref_axis',(1.,0.,0.));
#16554=DIRECTION('',(1.,0.,0.));
#16555=DIRECTION('center_axis',(0.,0.,1.));
#16556=DIRECTION('ref_axis',(1.,0.,0.));
#16557=DIRECTION('',(-1.,0.,0.));
#16558=DIRECTION('center_axis',(0.,0.,1.));
#16559=DIRECTION('ref_axis',(1.,0.,0.));
#16560=DIRECTION('',(1.,0.,0.));
#16561=DIRECTION('center_axis',(0.,0.,1.));
#16562=DIRECTION('ref_axis',(1.,0.,0.));
#16563=DIRECTION('',(-1.,0.,0.));
#16564=DIRECTION('center_axis',(0.,0.,1.));
#16565=DIRECTION('ref_axis',(1.,0.,0.));
#16566=DIRECTION('',(1.,0.,0.));
#16567=DIRECTION('center_axis',(0.,0.,1.));
#16568=DIRECTION('ref_axis',(1.,0.,0.));
#16569=DIRECTION('',(-1.,0.,0.));
#16570=DIRECTION('',(1.,0.,0.));
#16571=DIRECTION('',(-1.,0.,0.));
#16572=DIRECTION('center_axis',(0.,1.,0.));
#16573=DIRECTION('ref_axis',(-1.,0.,0.));
#16574=DIRECTION('',(1.,0.,0.));
#16575=DIRECTION('center_axis',(0.,-1.,0.));
#16576=DIRECTION('ref_axis',(1.,0.,0.));
#16577=DIRECTION('',(-1.,0.,0.));
#16578=DIRECTION('center_axis',(0.,0.,1.));
#16579=DIRECTION('ref_axis',(-1.,-1.22464679914735E-16,0.));
#16580=DIRECTION('',(0.,0.,1.));
#16581=DIRECTION('',(0.,0.,1.));
#16582=DIRECTION('center_axis',(0.,0.,-1.));
#16583=DIRECTION('ref_axis',(1.,0.,0.));
#16584=DIRECTION('center_axis',(0.,0.,1.));
#16585=DIRECTION('ref_axis',(1.,0.,0.));
#16586=DIRECTION('',(0.,0.,1.));
#16587=DIRECTION('center_axis',(0.,0.,-1.));
#16588=DIRECTION('ref_axis',(1.,0.,0.));
#16589=DIRECTION('',(0.,0.,1.));
#16590=DIRECTION('center_axis',(0.,1.,0.));
#16591=DIRECTION('ref_axis',(-1.,0.,0.));
#16592=DIRECTION('',(1.,0.,0.));
#16593=DIRECTION('center_axis',(0.,-1.,0.));
#16594=DIRECTION('ref_axis',(1.,0.,0.));
#16595=DIRECTION('',(-1.,0.,0.));
#16596=DIRECTION('center_axis',(0.,0.,1.));
#16597=DIRECTION('ref_axis',(-1.,-1.22464679914735E-16,0.));
#16598=DIRECTION('',(0.,0.,-1.));
#16599=DIRECTION('center_axis',(0.,0.,-1.));
#16600=DIRECTION('ref_axis',(1.,0.,0.));
#16601=DIRECTION('',(0.,0.,1.));
#16602=DIRECTION('',(0.,0.,1.));
#16603=DIRECTION('center_axis',(0.,0.,-1.));
#16604=DIRECTION('ref_axis',(1.,0.,0.));
#16605=DIRECTION('',(0.,0.,1.));
#16606=DIRECTION('center_axis',(0.,0.,-1.));
#16607=DIRECTION('ref_axis',(1.,0.,0.));
#16608=DIRECTION('center_axis',(0.,0.,1.));
#16609=DIRECTION('ref_axis',(1.,0.,0.));
#16610=DIRECTION('',(0.,0.,1.));
#16611=DIRECTION('center_axis',(0.,0.,-1.));
#16612=DIRECTION('ref_axis',(1.,0.,0.));
#16613=DIRECTION('',(0.,0.,1.));
#16614=DIRECTION('center_axis',(0.,1.,0.));
#16615=DIRECTION('ref_axis',(-1.,0.,0.));
#16616=DIRECTION('',(1.,0.,0.));
#16617=DIRECTION('center_axis',(0.,-1.,0.));
#16618=DIRECTION('ref_axis',(1.,0.,0.));
#16619=DIRECTION('',(-1.,0.,0.));
#16620=DIRECTION('center_axis',(0.,0.,1.));
#16621=DIRECTION('ref_axis',(-1.,-1.22464679914735E-16,0.));
#16622=DIRECTION('',(0.,0.,-1.));
#16623=DIRECTION('center_axis',(0.,0.,-1.));
#16624=DIRECTION('ref_axis',(1.,0.,0.));
#16625=DIRECTION('',(0.,0.,1.));
#16626=DIRECTION('',(0.,0.,1.));
#16627=DIRECTION('center_axis',(0.,0.,-1.));
#16628=DIRECTION('ref_axis',(1.,0.,0.));
#16629=DIRECTION('',(0.,0.,1.));
#16630=DIRECTION('center_axis',(0.,0.,-1.));
#16631=DIRECTION('ref_axis',(1.,0.,0.));
#16632=DIRECTION('center_axis',(0.,0.,1.));
#16633=DIRECTION('ref_axis',(1.,0.,0.));
#16634=DIRECTION('',(0.,0.,1.));
#16635=DIRECTION('center_axis',(0.,0.,-1.));
#16636=DIRECTION('ref_axis',(1.,0.,0.));
#16637=DIRECTION('',(0.,0.,1.));
#16638=DIRECTION('center_axis',(0.,1.,0.));
#16639=DIRECTION('ref_axis',(-1.,0.,0.));
#16640=DIRECTION('',(1.,0.,0.));
#16641=DIRECTION('center_axis',(0.,-1.,0.));
#16642=DIRECTION('ref_axis',(1.,0.,0.));
#16643=DIRECTION('',(-1.,0.,0.));
#16644=DIRECTION('center_axis',(0.,0.,1.));
#16645=DIRECTION('ref_axis',(-1.,5.66553889764798E-16,0.));
#16646=DIRECTION('center_axis',(0.,0.,-1.));
#16647=DIRECTION('ref_axis',(1.,0.,0.));
#16648=DIRECTION('center_axis',(0.,0.,1.));
#16649=DIRECTION('ref_axis',(1.,0.,0.));
#16650=DIRECTION('center_axis',(0.,0.,1.));
#16651=DIRECTION('ref_axis',(1.,0.,0.));
#16652=DIRECTION('center_axis',(0.,0.,1.));
#16653=DIRECTION('ref_axis',(1.,0.,0.));
#16654=DIRECTION('center_axis',(0.,0.,1.));
#16655=DIRECTION('ref_axis',(1.,0.,0.));
#16656=DIRECTION('',(0.,0.,1.));
#16657=DIRECTION('center_axis',(0.,0.,-1.));
#16658=DIRECTION('ref_axis',(1.,0.,0.));
#16659=DIRECTION('center_axis',(0.,0.,1.));
#16660=DIRECTION('ref_axis',(1.,0.,0.));
#16661=DIRECTION('center_axis',(0.,0.,1.));
#16662=DIRECTION('ref_axis',(1.,0.,0.));
#16663=DIRECTION('center_axis',(0.,0.,1.));
#16664=DIRECTION('ref_axis',(1.,0.,0.));
#16665=DIRECTION('',(0.,0.,1.));
#16666=DIRECTION('center_axis',(0.,0.,-1.));
#16667=DIRECTION('ref_axis',(1.,0.,0.));
#16668=DIRECTION('center_axis',(0.,0.,1.));
#16669=DIRECTION('ref_axis',(1.,0.,0.));
#16670=DIRECTION('center_axis',(0.,0.,1.));
#16671=DIRECTION('ref_axis',(-1.,-3.21624529935327E-16,0.));
#16672=DIRECTION('center_axis',(0.,0.,-1.));
#16673=DIRECTION('ref_axis',(1.,0.,0.));
#16674=DIRECTION('center_axis',(0.,0.,1.));
#16675=DIRECTION('ref_axis',(1.,0.,0.));
#16676=DIRECTION('center_axis',(0.,0.,1.));
#16677=DIRECTION('ref_axis',(1.,0.,0.));
#16678=DIRECTION('center_axis',(0.,1.,0.));
#16679=DIRECTION('ref_axis',(-1.,0.,0.));
#16680=DIRECTION('',(0.,0.,1.));
#16681=DIRECTION('',(-1.,0.,0.));
#16682=DIRECTION('',(0.,0.,1.));
#16683=DIRECTION('center_axis',(1.,0.,0.));
#16684=DIRECTION('ref_axis',(0.,1.,0.));
#16685=DIRECTION('',(0.,1.,0.));
#16686=DIRECTION('',(0.,0.,1.));
#16687=DIRECTION('center_axis',(0.,-1.,0.));
#16688=DIRECTION('ref_axis',(1.,0.,0.));
#16689=DIRECTION('',(1.,0.,0.));
#16690=DIRECTION('',(0.,0.,1.));
#16691=DIRECTION('center_axis',(-1.,0.,0.));
#16692=DIRECTION('ref_axis',(0.,-1.,0.));
#16693=DIRECTION('',(0.,-1.,0.));
#16694=DIRECTION('center_axis',(0.,0.,1.));
#16695=DIRECTION('ref_axis',(1.,0.,0.));
#16696=DIRECTION('axis',(0.,0.,1.));
#16697=DIRECTION('refdir',(1.,0.,0.));
#16698=DIRECTION('center_axis',(0.,1.,0.));
#16699=DIRECTION('ref_axis',(-1.,0.,0.));
#16700=DIRECTION('',(-1.,0.,0.));
#16701=DIRECTION('',(0.,0.,1.));
#16702=DIRECTION('',(-1.,0.,0.));
#16703=DIRECTION('',(0.,0.,1.));
#16704=DIRECTION('center_axis',(1.,0.,0.));
#16705=DIRECTION('ref_axis',(0.,1.,0.));
#16706=DIRECTION('',(0.,1.,0.));
#16707=DIRECTION('',(0.,1.,0.));
#16708=DIRECTION('',(0.,0.,1.));
#16709=DIRECTION('center_axis',(0.,-1.,0.));
#16710=DIRECTION('ref_axis',(1.,0.,0.));
#16711=DIRECTION('',(1.,0.,0.));
#16712=DIRECTION('',(1.,0.,0.));
#16713=DIRECTION('',(0.,0.,1.));
#16714=DIRECTION('center_axis',(-1.,0.,0.));
#16715=DIRECTION('ref_axis',(0.,-1.,0.));
#16716=DIRECTION('',(0.,-1.,0.));
#16717=DIRECTION('',(0.,-1.,0.));
#16718=DIRECTION('center_axis',(0.,0.,1.));
#16719=DIRECTION('ref_axis',(1.,0.,0.));
#16720=DIRECTION('center_axis',(0.,0.,1.));
#16721=DIRECTION('ref_axis',(1.,0.,0.));
#16722=DIRECTION('axis',(0.,0.,1.));
#16723=DIRECTION('refdir',(1.,0.,0.));
#16724=DIRECTION('center_axis',(0.,1.,0.));
#16725=DIRECTION('ref_axis',(-1.,0.,0.));
#16726=DIRECTION('',(-1.,0.,0.));
#16727=DIRECTION('',(0.,0.,1.));
#16728=DIRECTION('',(-1.,0.,0.));
#16729=DIRECTION('',(0.,0.,1.));
#16730=DIRECTION('center_axis',(1.,0.,0.));
#16731=DIRECTION('ref_axis',(0.,1.,0.));
#16732=DIRECTION('',(0.,1.,0.));
#16733=DIRECTION('',(0.,1.,0.));
#16734=DIRECTION('',(0.,0.,1.));
#16735=DIRECTION('center_axis',(0.,-1.,0.));
#16736=DIRECTION('ref_axis',(1.,0.,0.));
#16737=DIRECTION('',(1.,0.,0.));
#16738=DIRECTION('',(1.,0.,0.));
#16739=DIRECTION('',(0.,0.,1.));
#16740=DIRECTION('center_axis',(-1.,0.,0.));
#16741=DIRECTION('ref_axis',(0.,-1.,0.));
#16742=DIRECTION('',(0.,-1.,0.));
#16743=DIRECTION('',(0.,-1.,0.));
#16744=DIRECTION('center_axis',(0.,0.,1.));
#16745=DIRECTION('ref_axis',(1.,0.,0.));
#16746=DIRECTION('center_axis',(0.,0.,1.));
#16747=DIRECTION('ref_axis',(1.,0.,0.));
#16748=DIRECTION('axis',(0.,0.,1.));
#16749=DIRECTION('refdir',(1.,0.,0.));
#16750=DIRECTION('center_axis',(0.,1.,0.));
#16751=DIRECTION('ref_axis',(1.,0.,0.));
#16752=DIRECTION('center_axis',(0.,1.,0.));
#16753=DIRECTION('ref_axis',(1.,0.,0.));
#16754=DIRECTION('',(0.,1.,0.));
#16755=DIRECTION('center_axis',(0.,-1.,0.));
#16756=DIRECTION('ref_axis',(1.,0.,0.));
#16757=DIRECTION('center_axis',(0.,1.,0.));
#16758=DIRECTION('ref_axis',(1.,0.,0.));
#16759=DIRECTION('center_axis',(0.,1.,0.));
#16760=DIRECTION('ref_axis',(1.,0.,0.));
#16761=DIRECTION('',(0.,1.,0.));
#16762=DIRECTION('center_axis',(0.,-1.,0.));
#16763=DIRECTION('ref_axis',(1.,0.,0.));
#16764=DIRECTION('center_axis',(0.,1.,0.));
#16765=DIRECTION('ref_axis',(1.,0.,0.));
#16766=DIRECTION('center_axis',(0.,1.,0.));
#16767=DIRECTION('ref_axis',(1.,0.,0.));
#16768=DIRECTION('',(0.,1.,0.));
#16769=DIRECTION('center_axis',(0.,-1.,0.));
#16770=DIRECTION('ref_axis',(1.,0.,0.));
#16771=DIRECTION('center_axis',(0.,1.,0.));
#16772=DIRECTION('ref_axis',(1.,0.,0.));
#16773=DIRECTION('center_axis',(0.,1.,0.));
#16774=DIRECTION('ref_axis',(1.,0.,0.));
#16775=DIRECTION('',(0.,1.,0.));
#16776=DIRECTION('center_axis',(0.,-1.,0.));
#16777=DIRECTION('ref_axis',(1.,0.,0.));
#16778=DIRECTION('center_axis',(0.,1.,0.));
#16779=DIRECTION('ref_axis',(1.,0.,0.));
#16780=DIRECTION('center_axis',(0.,1.,0.));
#16781=DIRECTION('ref_axis',(1.,0.,0.));
#16782=DIRECTION('',(0.,1.,0.));
#16783=DIRECTION('center_axis',(0.,-1.,0.));
#16784=DIRECTION('ref_axis',(1.,0.,0.));
#16785=DIRECTION('center_axis',(0.,0.,1.));
#16786=DIRECTION('ref_axis',(1.,0.,0.));
#16787=DIRECTION('center_axis',(0.,0.,1.));
#16788=DIRECTION('ref_axis',(1.,0.,0.));
#16789=DIRECTION('',(0.,0.,1.));
#16790=DIRECTION('center_axis',(0.,0.,-1.));
#16791=DIRECTION('ref_axis',(1.,0.,0.));
#16792=DIRECTION('center_axis',(0.,0.,1.));
#16793=DIRECTION('ref_axis',(1.,0.,0.));
#16794=DIRECTION('center_axis',(0.,0.,1.));
#16795=DIRECTION('ref_axis',(1.,0.,0.));
#16796=DIRECTION('',(0.,0.,1.));
#16797=DIRECTION('center_axis',(0.,0.,-1.));
#16798=DIRECTION('ref_axis',(1.,0.,0.));
#16799=DIRECTION('center_axis',(0.,0.,1.));
#16800=DIRECTION('ref_axis',(1.,0.,0.));
#16801=DIRECTION('center_axis',(0.,0.,1.));
#16802=DIRECTION('ref_axis',(1.,0.,0.));
#16803=DIRECTION('',(0.,0.,1.));
#16804=DIRECTION('center_axis',(0.,0.,-1.));
#16805=DIRECTION('ref_axis',(1.,0.,0.));
#16806=DIRECTION('center_axis',(0.,0.,1.));
#16807=DIRECTION('ref_axis',(1.,0.,0.));
#16808=DIRECTION('center_axis',(0.,0.,1.));
#16809=DIRECTION('ref_axis',(1.,0.,0.));
#16810=DIRECTION('',(0.,0.,1.));
#16811=DIRECTION('center_axis',(0.,0.,-1.));
#16812=DIRECTION('ref_axis',(1.,0.,0.));
#16813=DIRECTION('center_axis',(0.,0.,1.));
#16814=DIRECTION('ref_axis',(1.,0.,0.));
#16815=DIRECTION('',(0.,1.,0.));
#16816=DIRECTION('',(-1.,0.,0.));
#16817=DIRECTION('',(0.,1.,0.));
#16818=DIRECTION('',(1.,0.,0.));
#16819=DIRECTION('center_axis',(0.,0.,1.));
#16820=DIRECTION('ref_axis',(1.,0.,0.));
#16821=DIRECTION('',(0.,-1.,0.));
#16822=DIRECTION('',(1.,0.,0.));
#16823=DIRECTION('',(0.,1.,0.));
#16824=DIRECTION('',(-1.,0.,0.));
#16825=DIRECTION('center_axis',(-1.,0.,0.));
#16826=DIRECTION('ref_axis',(0.,0.,1.));
#16827=DIRECTION('',(0.,0.,-1.));
#16828=DIRECTION('',(0.,0.,1.));
#16829=DIRECTION('',(0.,1.,0.));
#16830=DIRECTION('center_axis',(1.,0.,0.));
#16831=DIRECTION('ref_axis',(0.,0.,-1.));
#16832=DIRECTION('',(0.,0.,1.));
#16833=DIRECTION('',(0.,1.,0.));
#16834=DIRECTION('',(0.,0.,-1.));
#16835=DIRECTION('center_axis',(0.,-1.,0.));
#16836=DIRECTION('ref_axis',(1.,0.,0.));
#16837=DIRECTION('',(0.,0.,1.));
#16838=DIRECTION('',(1.,0.,0.));
#16839=DIRECTION('',(0.,0.,1.));
#16840=DIRECTION('',(1.,0.,0.));
#16841=DIRECTION('center_axis',(1.,0.,0.));
#16842=DIRECTION('ref_axis',(0.,1.,0.));
#16843=DIRECTION('',(0.,0.,1.));
#16844=DIRECTION('',(0.,1.,0.));
#16845=DIRECTION('center_axis',(0.,1.,0.));
#16846=DIRECTION('ref_axis',(-1.,0.,0.));
#16847=DIRECTION('',(0.,0.,1.));
#16848=DIRECTION('',(-1.,0.,0.));
#16849=DIRECTION('',(-1.,0.,0.));
#16850=DIRECTION('center_axis',(-1.,0.,0.));
#16851=DIRECTION('ref_axis',(0.,-1.,0.));
#16852=DIRECTION('',(0.,-1.,0.));
#16853=DIRECTION('center_axis',(0.,0.,1.));
#16854=DIRECTION('ref_axis',(1.,0.,0.));
#16855=DIRECTION('center_axis',(0.,0.,1.));
#16856=DIRECTION('ref_axis',(1.,0.,0.));
#16857=DIRECTION('axis',(0.,0.,1.));
#16858=DIRECTION('refdir',(1.,0.,0.));
#16859=DIRECTION('center_axis',(0.,1.,0.));
#16860=DIRECTION('ref_axis',(1.,0.,0.));
#16861=DIRECTION('center_axis',(0.,-1.,0.));
#16862=DIRECTION('ref_axis',(1.,0.,0.));
#16863=DIRECTION('',(0.,-1.,0.));
#16864=DIRECTION('center_axis',(0.,-1.,0.));
#16865=DIRECTION('ref_axis',(1.,0.,0.));
#16866=DIRECTION('center_axis',(0.,1.,0.));
#16867=DIRECTION('ref_axis',(1.,0.,0.));
#16868=DIRECTION('center_axis',(0.,1.,0.));
#16869=DIRECTION('ref_axis',(1.,0.,0.));
#16870=DIRECTION('',(0.,-1.,0.));
#16871=DIRECTION('center_axis',(0.,1.,0.));
#16872=DIRECTION('ref_axis',(1.,0.,0.));
#16873=DIRECTION('center_axis',(0.,1.,0.));
#16874=DIRECTION('ref_axis',(1.,0.,0.));
#16875=DIRECTION('center_axis',(0.,1.,0.));
#16876=DIRECTION('ref_axis',(1.,0.,0.));
#16877=DIRECTION('axis',(0.,0.,1.));
#16878=DIRECTION('refdir',(1.,0.,0.));
#16879=DIRECTION('center_axis',(0.,1.,0.));
#16880=DIRECTION('ref_axis',(0.707106781186546,0.,0.707106781186549));
#16881=DIRECTION('',(0.,1.,0.));
#16882=DIRECTION('center_axis',(0.,1.,0.));
#16883=DIRECTION('ref_axis',(1.,0.,0.));
#16884=DIRECTION('',(0.,-1.,0.));
#16885=DIRECTION('center_axis',(0.,-1.,0.));
#16886=DIRECTION('ref_axis',(1.,0.,0.));
#16887=DIRECTION('center_axis',(0.,1.,0.));
#16888=DIRECTION('ref_axis',(0.707106781186547,0.,-0.707106781186548));
#16889=DIRECTION('',(0.,1.,0.));
#16890=DIRECTION('center_axis',(0.,1.,0.));
#16891=DIRECTION('ref_axis',(1.,0.,0.));
#16892=DIRECTION('',(0.,-1.,0.));
#16893=DIRECTION('center_axis',(0.,-1.,0.));
#16894=DIRECTION('ref_axis',(1.,0.,0.));
#16895=DIRECTION('center_axis',(0.,1.,0.));
#16896=DIRECTION('ref_axis',(-0.707106781186552,0.,-0.707106781186543));
#16897=DIRECTION('',(0.,1.,0.));
#16898=DIRECTION('center_axis',(0.,1.,0.));
#16899=DIRECTION('ref_axis',(1.,0.,0.));
#16900=DIRECTION('',(0.,-1.,0.));
#16901=DIRECTION('center_axis',(0.,-1.,0.));
#16902=DIRECTION('ref_axis',(1.,0.,0.));
#16903=DIRECTION('center_axis',(0.,1.,0.));
#16904=DIRECTION('ref_axis',(-0.707106781186546,0.,0.707106781186549));
#16905=DIRECTION('',(0.,1.,0.));
#16906=DIRECTION('center_axis',(0.,1.,0.));
#16907=DIRECTION('ref_axis',(1.,0.,0.));
#16908=DIRECTION('',(0.,-1.,0.));
#16909=DIRECTION('center_axis',(0.,-1.,0.));
#16910=DIRECTION('ref_axis',(1.,0.,0.));
#16911=DIRECTION('center_axis',(0.,1.,0.));
#16912=DIRECTION('ref_axis',(1.,0.,0.));
#16913=DIRECTION('center_axis',(0.,1.,0.));
#16914=DIRECTION('ref_axis',(1.,0.,0.));
#16915=DIRECTION('center_axis',(0.,1.,0.));
#16916=DIRECTION('ref_axis',(1.,0.,0.));
#16917=DIRECTION('center_axis',(0.,1.,0.));
#16918=DIRECTION('ref_axis',(1.,0.,0.));
#16919=DIRECTION('center_axis',(0.,1.,0.));
#16920=DIRECTION('ref_axis',(1.,0.,0.));
#16921=DIRECTION('center_axis',(0.,-1.,0.));
#16922=DIRECTION('ref_axis',(1.,0.,0.));
#16923=DIRECTION('center_axis',(0.,1.,0.));
#16924=DIRECTION('ref_axis',(1.,0.,0.));
#16925=DIRECTION('center_axis',(0.,1.,0.));
#16926=DIRECTION('ref_axis',(1.,0.,0.));
#16927=DIRECTION('center_axis',(0.,1.,0.));
#16928=DIRECTION('ref_axis',(1.,0.,0.));
#16929=DIRECTION('center_axis',(0.,1.,0.));
#16930=DIRECTION('ref_axis',(1.,0.,0.));
#16931=DIRECTION('center_axis',(0.,1.,0.));
#16932=DIRECTION('ref_axis',(1.,0.,0.));
#16933=DIRECTION('center_axis',(0.,1.,0.));
#16934=DIRECTION('ref_axis',(1.,0.,0.));
#16935=DIRECTION('center_axis',(0.,1.,0.));
#16936=DIRECTION('ref_axis',(-1.,0.,-1.22464679914735E-16));
#16937=DIRECTION('center_axis',(0.,1.,0.));
#16938=DIRECTION('ref_axis',(1.,0.,0.));
#16939=DIRECTION('center_axis',(0.,1.,0.));
#16940=DIRECTION('ref_axis',(1.,0.,0.));
#16941=DIRECTION('center_axis',(0.,1.,0.));
#16942=DIRECTION('ref_axis',(1.,0.,0.));
#16943=DIRECTION('',(0.,-1.,0.));
#16944=DIRECTION('center_axis',(0.,-1.,0.));
#16945=DIRECTION('ref_axis',(1.,0.,0.));
#16946=DIRECTION('center_axis',(0.,1.,0.));
#16947=DIRECTION('ref_axis',(1.,0.,0.));
#16948=DIRECTION('center_axis',(0.,-1.,0.));
#16949=DIRECTION('ref_axis',(1.,0.,0.));
#16950=DIRECTION('center_axis',(0.,1.,0.));
#16951=DIRECTION('ref_axis',(1.,0.,0.));
#16952=DIRECTION('',(0.,-1.,0.));
#16953=DIRECTION('center_axis',(0.,1.,0.));
#16954=DIRECTION('ref_axis',(1.,0.,0.));
#16955=DIRECTION('axis',(0.,0.,1.));
#16956=DIRECTION('refdir',(1.,0.,0.));
#16957=DIRECTION('center_axis',(0.,1.,0.));
#16958=DIRECTION('ref_axis',(0.707106781186546,0.,0.707106781186549));
#16959=DIRECTION('',(0.,1.,0.));
#16960=DIRECTION('center_axis',(0.,1.,0.));
#16961=DIRECTION('ref_axis',(1.,0.,0.));
#16962=DIRECTION('',(0.,-1.,0.));
#16963=DIRECTION('center_axis',(0.,-1.,0.));
#16964=DIRECTION('ref_axis',(1.,0.,0.));
#16965=DIRECTION('center_axis',(0.,1.,0.));
#16966=DIRECTION('ref_axis',(0.707106781186547,0.,-0.707106781186548));
#16967=DIRECTION('',(0.,1.,0.));
#16968=DIRECTION('center_axis',(0.,1.,0.));
#16969=DIRECTION('ref_axis',(1.,0.,0.));
#16970=DIRECTION('',(0.,-1.,0.));
#16971=DIRECTION('center_axis',(0.,-1.,0.));
#16972=DIRECTION('ref_axis',(1.,0.,0.));
#16973=DIRECTION('center_axis',(0.,1.,0.));
#16974=DIRECTION('ref_axis',(-0.707106781186552,0.,-0.707106781186543));
#16975=DIRECTION('',(0.,1.,0.));
#16976=DIRECTION('center_axis',(0.,1.,0.));
#16977=DIRECTION('ref_axis',(1.,0.,0.));
#16978=DIRECTION('',(0.,-1.,0.));
#16979=DIRECTION('center_axis',(0.,-1.,0.));
#16980=DIRECTION('ref_axis',(1.,0.,0.));
#16981=DIRECTION('center_axis',(0.,1.,0.));
#16982=DIRECTION('ref_axis',(-0.707106781186546,0.,0.707106781186549));
#16983=DIRECTION('',(0.,1.,0.));
#16984=DIRECTION('center_axis',(0.,1.,0.));
#16985=DIRECTION('ref_axis',(1.,0.,0.));
#16986=DIRECTION('',(0.,-1.,0.));
#16987=DIRECTION('center_axis',(0.,-1.,0.));
#16988=DIRECTION('ref_axis',(1.,0.,0.));
#16989=DIRECTION('center_axis',(0.,1.,0.));
#16990=DIRECTION('ref_axis',(1.,0.,0.));
#16991=DIRECTION('center_axis',(0.,1.,0.));
#16992=DIRECTION('ref_axis',(1.,0.,0.));
#16993=DIRECTION('center_axis',(0.,1.,0.));
#16994=DIRECTION('ref_axis',(1.,0.,0.));
#16995=DIRECTION('center_axis',(0.,1.,0.));
#16996=DIRECTION('ref_axis',(1.,0.,0.));
#16997=DIRECTION('center_axis',(0.,1.,0.));
#16998=DIRECTION('ref_axis',(1.,0.,0.));
#16999=DIRECTION('center_axis',(0.,1.,0.));
#17000=DIRECTION('ref_axis',(1.,0.,0.));
#17001=DIRECTION('center_axis',(0.,1.,0.));
#17002=DIRECTION('ref_axis',(1.,0.,0.));
#17003=DIRECTION('center_axis',(0.,1.,0.));
#17004=DIRECTION('ref_axis',(1.,0.,0.));
#17005=DIRECTION('center_axis',(0.,1.,0.));
#17006=DIRECTION('ref_axis',(1.,0.,0.));
#17007=DIRECTION('center_axis',(0.,1.,0.));
#17008=DIRECTION('ref_axis',(1.,0.,0.));
#17009=DIRECTION('center_axis',(0.,1.,0.));
#17010=DIRECTION('ref_axis',(1.,0.,0.));
#17011=DIRECTION('center_axis',(0.,1.,0.));
#17012=DIRECTION('ref_axis',(1.,0.,0.));
#17013=DIRECTION('center_axis',(0.,1.,0.));
#17014=DIRECTION('ref_axis',(-1.,0.,-1.22464679914735E-16));
#17015=DIRECTION('center_axis',(0.,1.,0.));
#17016=DIRECTION('ref_axis',(1.,0.,0.));
#17017=DIRECTION('center_axis',(0.,1.,0.));
#17018=DIRECTION('ref_axis',(1.,0.,0.));
#17019=DIRECTION('',(0.,-1.,0.));
#17020=DIRECTION('center_axis',(0.,1.,0.));
#17021=DIRECTION('ref_axis',(1.,0.,0.));
#17022=DIRECTION('center_axis',(0.,1.,0.));
#17023=DIRECTION('ref_axis',(1.,0.,0.));
#17024=DIRECTION('center_axis',(0.,-1.,0.));
#17025=DIRECTION('ref_axis',(1.,0.,0.));
#17026=DIRECTION('center_axis',(0.,1.,0.));
#17027=DIRECTION('ref_axis',(1.,0.,0.));
#17028=DIRECTION('center_axis',(0.,-1.,0.));
#17029=DIRECTION('ref_axis',(1.,0.,0.));
#17030=DIRECTION('',(0.,-1.,0.));
#17031=DIRECTION('center_axis',(0.,1.,0.));
#17032=DIRECTION('ref_axis',(1.,0.,0.));
#17033=DIRECTION('axis',(0.,0.,1.));
#17034=DIRECTION('refdir',(1.,0.,0.));
#17035=DIRECTION('center_axis',(0.,1.,0.));
#17036=DIRECTION('ref_axis',(1.,0.,0.));
#17037=DIRECTION('',(0.,1.,0.));
#17038=DIRECTION('center_axis',(0.,1.,0.));
#17039=DIRECTION('ref_axis',(1.,0.,0.));
#17040=DIRECTION('',(0.,-1.,0.));
#17041=DIRECTION('center_axis',(0.,-1.,0.));
#17042=DIRECTION('ref_axis',(1.,0.,0.));
#17043=DIRECTION('center_axis',(0.,1.,0.));
#17044=DIRECTION('ref_axis',(1.,0.,0.));
#17045=DIRECTION('',(0.,-1.,0.));
#17046=DIRECTION('center_axis',(0.,-1.,0.));
#17047=DIRECTION('ref_axis',(1.,0.,0.));
#17048=DIRECTION('',(0.,1.,0.));
#17049=DIRECTION('center_axis',(0.,1.,0.));
#17050=DIRECTION('ref_axis',(1.,0.,0.));
#17051=DIRECTION('center_axis',(0.,1.,0.));
#17052=DIRECTION('ref_axis',(1.,0.,0.));
#17053=DIRECTION('',(0.,0.,1.));
#17054=DIRECTION('center_axis',(0.,1.,0.));
#17055=DIRECTION('ref_axis',(1.,0.,0.));
#17056=DIRECTION('',(0.,0.,-1.));
#17057=DIRECTION('',(-1.,0.,0.));
#17058=DIRECTION('center_axis',(0.,1.,0.));
#17059=DIRECTION('ref_axis',(1.,0.,0.));
#17060=DIRECTION('center_axis',(0.,1.,0.));
#17061=DIRECTION('ref_axis',(1.,0.,0.));
#17062=DIRECTION('center_axis',(0.,1.,0.));
#17063=DIRECTION('ref_axis',(1.,0.,0.));
#17064=DIRECTION('center_axis',(0.,1.,0.));
#17065=DIRECTION('ref_axis',(1.,0.,0.));
#17066=DIRECTION('center_axis',(0.,1.,0.));
#17067=DIRECTION('ref_axis',(1.,0.,0.));
#17068=DIRECTION('center_axis',(0.,1.,0.));
#17069=DIRECTION('ref_axis',(1.,0.,0.));
#17070=DIRECTION('',(0.,-1.,0.));
#17071=DIRECTION('center_axis',(0.,-1.,0.));
#17072=DIRECTION('ref_axis',(1.,0.,0.));
#17073=DIRECTION('',(0.,1.,0.));
#17074=DIRECTION('center_axis',(1.,0.,0.));
#17075=DIRECTION('ref_axis',(0.,1.,0.));
#17076=DIRECTION('',(0.,0.,1.));
#17077=DIRECTION('',(0.,1.,0.));
#17078=DIRECTION('',(0.,0.,1.));
#17079=DIRECTION('',(0.,1.,0.));
#17080=DIRECTION('',(0.,0.,1.));
#17081=DIRECTION('center_axis',(0.,0.,1.));
#17082=DIRECTION('ref_axis',(1.,0.,0.));
#17083=DIRECTION('',(-1.,0.,0.));
#17084=DIRECTION('',(0.,-1.,0.));
#17085=DIRECTION('',(1.,0.,0.));
#17086=DIRECTION('',(-1.,0.,0.));
#17087=DIRECTION('center_axis',(0.,1.,0.));
#17088=DIRECTION('ref_axis',(-1.,0.,0.));
#17089=DIRECTION('center_axis',(0.,1.,0.));
#17090=DIRECTION('ref_axis',(-1.,0.,0.));
#17091=DIRECTION('',(0.,0.,1.));
#17092=DIRECTION('center_axis',(0.,1.,0.));
#17093=DIRECTION('ref_axis',(1.,0.,0.));
#17094=DIRECTION('center_axis',(0.,1.,0.));
#17095=DIRECTION('ref_axis',(1.,0.,0.));
#17096=DIRECTION('',(0.,1.,0.));
#17097=DIRECTION('center_axis',(0.,1.,0.));
#17098=DIRECTION('ref_axis',(1.,0.,0.));
#17099=DIRECTION('center_axis',(0.,1.,0.));
#17100=DIRECTION('ref_axis',(1.,0.,0.));
#17101=DIRECTION('',(0.,1.,0.));
#17102=DIRECTION('center_axis',(0.,1.,0.));
#17103=DIRECTION('ref_axis',(1.,0.,0.));
#17104=DIRECTION('center_axis',(0.,1.,0.));
#17105=DIRECTION('ref_axis',(1.,0.,0.));
#17106=DIRECTION('',(0.,1.,0.));
#17107=DIRECTION('center_axis',(0.,1.,0.));
#17108=DIRECTION('ref_axis',(1.,0.,0.));
#17109=DIRECTION('center_axis',(0.,1.,0.));
#17110=DIRECTION('ref_axis',(1.,0.,0.));
#17111=DIRECTION('',(0.,1.,0.));
#17112=DIRECTION('center_axis',(0.,1.,0.));
#17113=DIRECTION('ref_axis',(1.,0.,0.));
#17114=DIRECTION('center_axis',(0.,1.,0.));
#17115=DIRECTION('ref_axis',(1.,0.,0.));
#17116=DIRECTION('',(0.,1.,0.));
#17117=DIRECTION('center_axis',(0.,0.,1.));
#17118=DIRECTION('ref_axis',(1.,0.,0.));
#17119=DIRECTION('center_axis',(0.,0.,1.));
#17120=DIRECTION('ref_axis',(1.,0.,0.));
#17121=DIRECTION('',(0.,0.,1.));
#17122=DIRECTION('center_axis',(0.,0.,-1.));
#17123=DIRECTION('ref_axis',(1.,0.,0.));
#17124=DIRECTION('center_axis',(0.,0.,1.));
#17125=DIRECTION('ref_axis',(1.,0.,0.));
#17126=DIRECTION('center_axis',(0.,0.,1.));
#17127=DIRECTION('ref_axis',(1.,0.,0.));
#17128=DIRECTION('',(0.,0.,1.));
#17129=DIRECTION('center_axis',(0.,0.,-1.));
#17130=DIRECTION('ref_axis',(1.,0.,0.));
#17131=DIRECTION('center_axis',(0.,0.,1.));
#17132=DIRECTION('ref_axis',(1.,0.,0.));
#17133=DIRECTION('center_axis',(0.,0.,1.));
#17134=DIRECTION('ref_axis',(1.,0.,0.));
#17135=DIRECTION('',(0.,0.,1.));
#17136=DIRECTION('center_axis',(0.,0.,-1.));
#17137=DIRECTION('ref_axis',(1.,0.,0.));
#17138=DIRECTION('center_axis',(0.,0.,1.));
#17139=DIRECTION('ref_axis',(1.,0.,0.));
#17140=DIRECTION('center_axis',(0.,0.,1.));
#17141=DIRECTION('ref_axis',(1.,0.,0.));
#17142=DIRECTION('',(0.,0.,1.));
#17143=DIRECTION('center_axis',(0.,0.,-1.));
#17144=DIRECTION('ref_axis',(1.,0.,0.));
#17145=DIRECTION('center_axis',(0.,0.,1.));
#17146=DIRECTION('ref_axis',(1.,0.,0.));
#17147=DIRECTION('',(-1.,0.,0.));
#17148=DIRECTION('',(0.,1.,0.));
#17149=DIRECTION('',(1.,0.,0.));
#17150=DIRECTION('center_axis',(0.,0.,1.));
#17151=DIRECTION('ref_axis',(1.,0.,0.));
#17152=DIRECTION('',(0.,-1.,0.));
#17153=DIRECTION('',(1.,0.,0.));
#17154=DIRECTION('',(0.,1.,0.));
#17155=DIRECTION('',(-1.,0.,0.));
#17156=DIRECTION('center_axis',(-1.,0.,0.));
#17157=DIRECTION('ref_axis',(0.,0.,1.));
#17158=DIRECTION('',(0.,0.,-1.));
#17159=DIRECTION('',(0.,0.,1.));
#17160=DIRECTION('',(0.,1.,0.));
#17161=DIRECTION('center_axis',(1.,0.,0.));
#17162=DIRECTION('ref_axis',(0.,0.,-1.));
#17163=DIRECTION('',(0.,0.,1.));
#17164=DIRECTION('',(0.,1.,0.));
#17165=DIRECTION('',(0.,0.,-1.));
#17166=DIRECTION('center_axis',(0.,-1.,0.));
#17167=DIRECTION('ref_axis',(1.,0.,0.));
#17168=DIRECTION('',(0.,0.,1.));
#17169=DIRECTION('',(1.,0.,0.));
#17170=DIRECTION('center_axis',(0.,1.,0.));
#17171=DIRECTION('ref_axis',(-1.,0.,0.));
#17172=DIRECTION('',(-1.,0.,0.));
#17173=DIRECTION('',(0.,0.,1.));
#17174=DIRECTION('center_axis',(-1.,0.,0.));
#17175=DIRECTION('ref_axis',(0.,-1.,0.));
#17176=DIRECTION('center_axis',(0.,0.,1.));
#17177=DIRECTION('ref_axis',(1.,0.,0.));
#17178=DIRECTION('axis',(0.,0.,1.));
#17179=DIRECTION('refdir',(1.,0.,0.));
#17180=DIRECTION('center_axis',(0.,0.,1.));
#17181=DIRECTION('ref_axis',(1.,0.,0.));
#17182=DIRECTION('center_axis',(0.,0.,-1.));
#17183=DIRECTION('ref_axis',(1.,0.,0.));
#17184=DIRECTION('',(0.,0.,-1.));
#17185=DIRECTION('center_axis',(0.,0.,-1.));
#17186=DIRECTION('ref_axis',(1.,0.,0.));
#17187=DIRECTION('center_axis',(0.,0.,1.));
#17188=DIRECTION('ref_axis',(1.,0.,0.));
#17189=DIRECTION('center_axis',(0.,0.,1.));
#17190=DIRECTION('ref_axis',(1.,0.,0.));
#17191=DIRECTION('',(0.,0.,-1.));
#17192=DIRECTION('center_axis',(0.,0.,1.));
#17193=DIRECTION('ref_axis',(1.,0.,0.));
#17194=DIRECTION('center_axis',(0.,0.,1.));
#17195=DIRECTION('ref_axis',(1.,0.,0.));
#17196=DIRECTION('center_axis',(0.,0.,1.));
#17197=DIRECTION('ref_axis',(1.,0.,0.));
#17198=DIRECTION('axis',(0.,0.,1.));
#17199=DIRECTION('refdir',(1.,0.,0.));
#17200=DIRECTION('center_axis',(0.,0.,1.));
#17201=DIRECTION('ref_axis',(1.,0.,0.));
#17202=DIRECTION('center_axis',(0.,0.,-1.));
#17203=DIRECTION('ref_axis',(1.,0.,0.));
#17204=DIRECTION('',(0.,0.,-1.));
#17205=DIRECTION('center_axis',(0.,0.,-1.));
#17206=DIRECTION('ref_axis',(1.,0.,0.));
#17207=DIRECTION('center_axis',(0.,0.,1.));
#17208=DIRECTION('ref_axis',(1.,0.,0.));
#17209=DIRECTION('center_axis',(0.,0.,1.));
#17210=DIRECTION('ref_axis',(1.,0.,0.));
#17211=DIRECTION('',(0.,0.,-1.));
#17212=DIRECTION('center_axis',(0.,0.,1.));
#17213=DIRECTION('ref_axis',(1.,0.,0.));
#17214=DIRECTION('center_axis',(0.,0.,1.));
#17215=DIRECTION('ref_axis',(1.,0.,0.));
#17216=DIRECTION('center_axis',(0.,0.,1.));
#17217=DIRECTION('ref_axis',(1.,0.,0.));
#17218=DIRECTION('axis',(0.,0.,1.));
#17219=DIRECTION('refdir',(1.,0.,0.));
#17220=DIRECTION('center_axis',(0.,0.,1.));
#17221=DIRECTION('ref_axis',(1.,0.,0.));
#17222=DIRECTION('center_axis',(0.,0.,-1.));
#17223=DIRECTION('ref_axis',(1.,0.,0.));
#17224=DIRECTION('',(0.,0.,-1.));
#17225=DIRECTION('center_axis',(0.,0.,-1.));
#17226=DIRECTION('ref_axis',(1.,0.,0.));
#17227=DIRECTION('center_axis',(0.,0.,1.));
#17228=DIRECTION('ref_axis',(1.,0.,0.));
#17229=DIRECTION('center_axis',(0.,0.,1.));
#17230=DIRECTION('ref_axis',(1.,0.,0.));
#17231=DIRECTION('',(0.,0.,-1.));
#17232=DIRECTION('center_axis',(0.,0.,1.));
#17233=DIRECTION('ref_axis',(1.,0.,0.));
#17234=DIRECTION('center_axis',(0.,0.,1.));
#17235=DIRECTION('ref_axis',(1.,0.,0.));
#17236=DIRECTION('center_axis',(0.,0.,1.));
#17237=DIRECTION('ref_axis',(1.,0.,0.));
#17238=DIRECTION('axis',(0.,0.,1.));
#17239=DIRECTION('refdir',(1.,0.,0.));
#17240=DIRECTION('center_axis',(0.,0.,1.));
#17241=DIRECTION('ref_axis',(1.,0.,0.));
#17242=DIRECTION('center_axis',(0.,0.,-1.));
#17243=DIRECTION('ref_axis',(1.,0.,0.));
#17244=DIRECTION('',(0.,0.,-1.));
#17245=DIRECTION('center_axis',(0.,0.,-1.));
#17246=DIRECTION('ref_axis',(1.,0.,0.));
#17247=DIRECTION('center_axis',(0.,0.,1.));
#17248=DIRECTION('ref_axis',(1.,0.,0.));
#17249=DIRECTION('center_axis',(0.,0.,1.));
#17250=DIRECTION('ref_axis',(1.,0.,0.));
#17251=DIRECTION('',(0.,0.,-1.));
#17252=DIRECTION('center_axis',(0.,0.,1.));
#17253=DIRECTION('ref_axis',(1.,0.,0.));
#17254=DIRECTION('center_axis',(0.,0.,1.));
#17255=DIRECTION('ref_axis',(1.,0.,0.));
#17256=DIRECTION('center_axis',(0.,0.,1.));
#17257=DIRECTION('ref_axis',(1.,0.,0.));
#17258=DIRECTION('axis',(0.,0.,1.));
#17259=DIRECTION('refdir',(1.,0.,0.));
#17260=DIRECTION('center_axis',(0.,1.,0.));
#17261=DIRECTION('ref_axis',(1.,0.,0.));
#17262=DIRECTION('center_axis',(0.,-1.,0.));
#17263=DIRECTION('ref_axis',(1.,0.,0.));
#17264=DIRECTION('',(0.,-1.,0.));
#17265=DIRECTION('center_axis',(0.,-1.,0.));
#17266=DIRECTION('ref_axis',(1.,0.,0.));
#17267=DIRECTION('center_axis',(0.,1.,0.));
#17268=DIRECTION('ref_axis',(1.,0.,0.));
#17269=DIRECTION('center_axis',(0.,1.,0.));
#17270=DIRECTION('ref_axis',(1.,0.,0.));
#17271=DIRECTION('',(0.,-1.,0.));
#17272=DIRECTION('center_axis',(0.,1.,0.));
#17273=DIRECTION('ref_axis',(1.,0.,0.));
#17274=DIRECTION('center_axis',(0.,1.,0.));
#17275=DIRECTION('ref_axis',(1.,0.,0.));
#17276=DIRECTION('center_axis',(0.,1.,0.));
#17277=DIRECTION('ref_axis',(1.,0.,0.));
#17278=DIRECTION('axis',(0.,0.,1.));
#17279=DIRECTION('refdir',(1.,0.,0.));
#17280=DIRECTION('center_axis',(0.,1.,0.));
#17281=DIRECTION('ref_axis',(0.707106781186546,0.,0.707106781186549));
#17282=DIRECTION('',(0.,1.,0.));
#17283=DIRECTION('center_axis',(0.,1.,0.));
#17284=DIRECTION('ref_axis',(1.,0.,0.));
#17285=DIRECTION('',(0.,-1.,0.));
#17286=DIRECTION('center_axis',(0.,-1.,0.));
#17287=DIRECTION('ref_axis',(1.,0.,0.));
#17288=DIRECTION('center_axis',(0.,1.,0.));
#17289=DIRECTION('ref_axis',(0.707106781186544,0.,-0.707106781186551));
#17290=DIRECTION('',(0.,1.,0.));
#17291=DIRECTION('center_axis',(0.,1.,0.));
#17292=DIRECTION('ref_axis',(1.,0.,0.));
#17293=DIRECTION('',(0.,-1.,0.));
#17294=DIRECTION('center_axis',(0.,-1.,0.));
#17295=DIRECTION('ref_axis',(1.,0.,0.));
#17296=DIRECTION('center_axis',(0.,1.,0.));
#17297=DIRECTION('ref_axis',(-0.707106781186548,0.,-0.707106781186547));
#17298=DIRECTION('',(0.,1.,0.));
#17299=DIRECTION('center_axis',(0.,1.,0.));
#17300=DIRECTION('ref_axis',(1.,0.,0.));
#17301=DIRECTION('',(0.,-1.,0.));
#17302=DIRECTION('center_axis',(0.,-1.,0.));
#17303=DIRECTION('ref_axis',(1.,0.,0.));
#17304=DIRECTION('center_axis',(0.,1.,0.));
#17305=DIRECTION('ref_axis',(-0.707106781186544,0.,0.707106781186551));
#17306=DIRECTION('',(0.,1.,0.));
#17307=DIRECTION('center_axis',(0.,1.,0.));
#17308=DIRECTION('ref_axis',(1.,0.,0.));
#17309=DIRECTION('',(0.,-1.,0.));
#17310=DIRECTION('center_axis',(0.,-1.,0.));
#17311=DIRECTION('ref_axis',(1.,0.,0.));
#17312=DIRECTION('center_axis',(0.,1.,0.));
#17313=DIRECTION('ref_axis',(1.,0.,0.));
#17314=DIRECTION('center_axis',(0.,1.,0.));
#17315=DIRECTION('ref_axis',(1.,0.,0.));
#17316=DIRECTION('center_axis',(0.,1.,0.));
#17317=DIRECTION('ref_axis',(1.,0.,0.));
#17318=DIRECTION('center_axis',(0.,1.,0.));
#17319=DIRECTION('ref_axis',(1.,0.,0.));
#17320=DIRECTION('center_axis',(0.,1.,0.));
#17321=DIRECTION('ref_axis',(1.,0.,0.));
#17322=DIRECTION('center_axis',(0.,-1.,0.));
#17323=DIRECTION('ref_axis',(1.,0.,0.));
#17324=DIRECTION('center_axis',(0.,1.,0.));
#17325=DIRECTION('ref_axis',(1.,0.,0.));
#17326=DIRECTION('center_axis',(0.,1.,0.));
#17327=DIRECTION('ref_axis',(1.,0.,0.));
#17328=DIRECTION('center_axis',(0.,1.,0.));
#17329=DIRECTION('ref_axis',(1.,0.,0.));
#17330=DIRECTION('center_axis',(0.,1.,0.));
#17331=DIRECTION('ref_axis',(1.,0.,0.));
#17332=DIRECTION('center_axis',(0.,1.,0.));
#17333=DIRECTION('ref_axis',(1.,0.,0.));
#17334=DIRECTION('center_axis',(0.,1.,0.));
#17335=DIRECTION('ref_axis',(1.,0.,0.));
#17336=DIRECTION('center_axis',(0.,1.,0.));
#17337=DIRECTION('ref_axis',(-1.,0.,-1.01064309961486E-15));
#17338=DIRECTION('center_axis',(0.,1.,0.));
#17339=DIRECTION('ref_axis',(1.,0.,0.));
#17340=DIRECTION('center_axis',(0.,1.,0.));
#17341=DIRECTION('ref_axis',(1.,0.,0.));
#17342=DIRECTION('center_axis',(0.,1.,0.));
#17343=DIRECTION('ref_axis',(1.,0.,0.));
#17344=DIRECTION('',(0.,-1.,0.));
#17345=DIRECTION('center_axis',(0.,-1.,0.));
#17346=DIRECTION('ref_axis',(1.,0.,0.));
#17347=DIRECTION('center_axis',(0.,1.,0.));
#17348=DIRECTION('ref_axis',(1.,0.,0.));
#17349=DIRECTION('center_axis',(0.,-1.,0.));
#17350=DIRECTION('ref_axis',(1.,0.,0.));
#17351=DIRECTION('center_axis',(0.,1.,0.));
#17352=DIRECTION('ref_axis',(1.,0.,0.));
#17353=DIRECTION('',(0.,-1.,0.));
#17354=DIRECTION('center_axis',(0.,1.,0.));
#17355=DIRECTION('ref_axis',(1.,0.,0.));
#17356=DIRECTION('axis',(0.,0.,1.));
#17357=DIRECTION('refdir',(1.,0.,0.));
#17358=DIRECTION('center_axis',(0.,1.,0.));
#17359=DIRECTION('ref_axis',(1.,0.,0.));
#17360=DIRECTION('',(0.,1.,0.));
#17361=DIRECTION('center_axis',(0.,1.,0.));
#17362=DIRECTION('ref_axis',(1.,0.,0.));
#17363=DIRECTION('',(0.,-1.,0.));
#17364=DIRECTION('center_axis',(0.,-1.,0.));
#17365=DIRECTION('ref_axis',(1.,0.,0.));
#17366=DIRECTION('center_axis',(0.,1.,0.));
#17367=DIRECTION('ref_axis',(1.,0.,0.));
#17368=DIRECTION('center_axis',(0.,-1.,0.));
#17369=DIRECTION('ref_axis',(1.,0.,0.));
#17370=DIRECTION('center_axis',(0.,1.,0.));
#17371=DIRECTION('ref_axis',(1.,0.,0.));
#17372=DIRECTION('center_axis',(0.,-1.,0.));
#17373=DIRECTION('ref_axis',(1.,0.,0.));
#17374=DIRECTION('center_axis',(0.,1.,0.));
#17375=DIRECTION('ref_axis',(1.,0.,0.));
#17376=DIRECTION('center_axis',(0.,-1.,0.));
#17377=DIRECTION('ref_axis',(1.,0.,0.));
#17378=DIRECTION('center_axis',(0.,1.,0.));
#17379=DIRECTION('ref_axis',(1.,0.,0.));
#17380=DIRECTION('center_axis',(0.,-1.,0.));
#17381=DIRECTION('ref_axis',(1.,0.,0.));
#17382=DIRECTION('center_axis',(0.,1.,0.));
#17383=DIRECTION('ref_axis',(1.,0.,0.));
#17384=DIRECTION('center_axis',(0.,1.,0.));
#17385=DIRECTION('ref_axis',(1.,0.,0.));
#17386=DIRECTION('',(0.,-1.,0.));
#17387=DIRECTION('center_axis',(0.,-1.,0.));
#17388=DIRECTION('ref_axis',(1.,0.,0.));
#17389=DIRECTION('',(0.,1.,0.));
#17390=DIRECTION('center_axis',(0.,1.,0.));
#17391=DIRECTION('ref_axis',(1.,0.,0.));
#17392=DIRECTION('center_axis',(0.,-1.,0.));
#17393=DIRECTION('ref_axis',(1.,0.,0.));
#17394=DIRECTION('center_axis',(0.,1.,0.));
#17395=DIRECTION('ref_axis',(1.,0.,0.));
#17396=DIRECTION('center_axis',(0.,-1.,0.));
#17397=DIRECTION('ref_axis',(1.,0.,0.));
#17398=DIRECTION('center_axis',(0.,1.,0.));
#17399=DIRECTION('ref_axis',(1.,0.,0.));
#17400=DIRECTION('center_axis',(0.,1.,0.));
#17401=DIRECTION('ref_axis',(-0.707106781186547,0.,-0.707106781186548));
#17402=DIRECTION('',(0.,-1.,0.));
#17403=DIRECTION('center_axis',(0.,-1.,0.));
#17404=DIRECTION('ref_axis',(1.,0.,0.));
#17405=DIRECTION('',(0.,1.,0.));
#17406=DIRECTION('center_axis',(0.,1.,0.));
#17407=DIRECTION('ref_axis',(1.,0.,0.));
#17408=DIRECTION('center_axis',(0.,-1.,0.));
#17409=DIRECTION('ref_axis',(1.,0.,0.));
#17410=DIRECTION('center_axis',(0.,1.,0.));
#17411=DIRECTION('ref_axis',(1.,0.,0.));
#17412=DIRECTION('center_axis',(0.,-1.,0.));
#17413=DIRECTION('ref_axis',(1.,0.,0.));
#17414=DIRECTION('center_axis',(0.,1.,0.));
#17415=DIRECTION('ref_axis',(1.,0.,0.));
#17416=DIRECTION('center_axis',(0.,1.,0.));
#17417=DIRECTION('ref_axis',(-0.707106781186548,0.,0.707106781186547));
#17418=DIRECTION('',(0.,-1.,0.));
#17419=DIRECTION('center_axis',(0.,-1.,0.));
#17420=DIRECTION('ref_axis',(1.,0.,0.));
#17421=DIRECTION('',(0.,1.,0.));
#17422=DIRECTION('center_axis',(0.,1.,0.));
#17423=DIRECTION('ref_axis',(0.707106781186545,0.,-0.70710678118655));
#17424=DIRECTION('',(0.,1.,0.));
#17425=DIRECTION('center_axis',(0.,1.,0.));
#17426=DIRECTION('ref_axis',(1.,0.,0.));
#17427=DIRECTION('',(0.,-1.,0.));
#17428=DIRECTION('center_axis',(0.,1.,0.));
#17429=DIRECTION('ref_axis',(-0.707106781186547,0.,-0.707106781186548));
#17430=DIRECTION('',(0.,1.,0.));
#17431=DIRECTION('center_axis',(0.,1.,0.));
#17432=DIRECTION('ref_axis',(1.,0.,0.));
#17433=DIRECTION('',(0.,-1.,0.));
#17434=DIRECTION('center_axis',(0.,1.,0.));
#17435=DIRECTION('ref_axis',(-0.707106781186544,0.,0.707106781186551));
#17436=DIRECTION('',(0.,1.,0.));
#17437=DIRECTION('center_axis',(0.,1.,0.));
#17438=DIRECTION('ref_axis',(1.,0.,0.));
#17439=DIRECTION('',(0.,-1.,0.));
#17440=DIRECTION('center_axis',(0.,1.,0.));
#17441=DIRECTION('ref_axis',(1.,0.,0.));
#17442=DIRECTION('center_axis',(0.,1.,0.));
#17443=DIRECTION('ref_axis',(1.,0.,0.));
#17444=DIRECTION('center_axis',(0.,1.,0.));
#17445=DIRECTION('ref_axis',(1.,0.,0.));
#17446=DIRECTION('',(0.,1.,0.));
#17447=DIRECTION('center_axis',(0.,1.,0.));
#17448=DIRECTION('ref_axis',(1.,0.,0.));
#17449=DIRECTION('center_axis',(0.,1.,0.));
#17450=DIRECTION('ref_axis',(1.,0.,0.));
#17451=DIRECTION('center_axis',(0.,1.,0.));
#17452=DIRECTION('ref_axis',(1.,0.,0.));
#17453=DIRECTION('center_axis',(0.,1.,0.));
#17454=DIRECTION('ref_axis',(1.,0.,0.));
#17455=DIRECTION('center_axis',(0.,-1.,0.));
#17456=DIRECTION('ref_axis',(1.,0.,0.));
#17457=DIRECTION('center_axis',(0.,1.,0.));
#17458=DIRECTION('ref_axis',(1.,0.,0.));
#17459=DIRECTION('center_axis',(0.,1.,0.));
#17460=DIRECTION('ref_axis',(1.,0.,0.));
#17461=DIRECTION('center_axis',(0.,1.,0.));
#17462=DIRECTION('ref_axis',(1.,0.,0.));
#17463=DIRECTION('center_axis',(0.,1.,0.));
#17464=DIRECTION('ref_axis',(1.,0.,0.));
#17465=DIRECTION('center_axis',(0.,1.,0.));
#17466=DIRECTION('ref_axis',(1.,0.,0.));
#17467=DIRECTION('center_axis',(0.,-1.,0.));
#17468=DIRECTION('ref_axis',(1.,0.,0.));
#17469=DIRECTION('center_axis',(0.,1.,0.));
#17470=DIRECTION('ref_axis',(1.,0.,0.));
#17471=DIRECTION('center_axis',(0.,1.,0.));
#17472=DIRECTION('ref_axis',(1.,0.,0.));
#17473=DIRECTION('center_axis',(0.,1.,0.));
#17474=DIRECTION('ref_axis',(0.707106781186544,0.,0.707106781186551));
#17475=DIRECTION('',(0.,-1.,0.));
#17476=DIRECTION('center_axis',(0.,1.,0.));
#17477=DIRECTION('ref_axis',(-1.,0.,-1.01064309961486E-15));
#17478=DIRECTION('center_axis',(0.,1.,0.));
#17479=DIRECTION('ref_axis',(1.,0.,0.));
#17480=DIRECTION('',(0.,-1.,0.));
#17481=DIRECTION('axis',(0.,0.,1.));
#17482=DIRECTION('refdir',(1.,0.,0.));
#17483=DIRECTION('center_axis',(-0.0913252028230577,0.,-0.99582112215464));
#17484=DIRECTION('ref_axis',(-0.99582112215464,0.,0.0913252028230577));
#17485=DIRECTION('',(-0.99582112215464,0.,0.0913252028230577));
#17486=DIRECTION('',(0.,-1.,0.));
#17487=DIRECTION('',(0.99582112215464,0.,-0.0913252028230577));
#17488=DIRECTION('',(0.,-1.,0.));
#17489=DIRECTION('center_axis',(-0.0913252028230577,0.,0.99582112215464));
#17490=DIRECTION('ref_axis',(0.99582112215464,0.,0.0913252028230577));
#17491=DIRECTION('',(0.99582112215464,0.,0.0913252028230577));
#17492=DIRECTION('',(0.,-1.,0.));
#17493=DIRECTION('',(-0.99582112215464,0.,-0.0913252028230577));
#17494=DIRECTION('',(0.,1.,0.));
#17495=DIRECTION('center_axis',(0.,1.,0.));
#17496=DIRECTION('ref_axis',(1.,0.,0.));
#17497=DIRECTION('',(0.99582112215464,0.,0.091325202823058));
#17498=DIRECTION('center_axis',(0.,1.,0.));
#17499=DIRECTION('ref_axis',(1.,0.,0.));
#17500=DIRECTION('',(-0.99582112215464,0.,0.0913252028230577));
#17501=DIRECTION('center_axis',(0.,1.,0.));
#17502=DIRECTION('ref_axis',(1.,0.,0.));
#17503=DIRECTION('center_axis',(0.,1.,0.));
#17504=DIRECTION('ref_axis',(1.,0.,0.));
#17505=DIRECTION('center_axis',(0.,1.,0.));
#17506=DIRECTION('ref_axis',(1.,0.,0.));
#17507=DIRECTION('center_axis',(0.,1.,0.));
#17508=DIRECTION('ref_axis',(-1.,0.,-1.22464679914735E-16));
#17509=DIRECTION('center_axis',(0.,-1.,0.));
#17510=DIRECTION('ref_axis',(1.,0.,0.));
#17511=DIRECTION('center_axis',(0.,1.,0.));
#17512=DIRECTION('ref_axis',(1.,0.,0.));
#17513=DIRECTION('center_axis',(0.,-1.,0.));
#17514=DIRECTION('ref_axis',(1.,0.,0.));
#17515=DIRECTION('center_axis',(0.,1.,0.));
#17516=DIRECTION('ref_axis',(1.,0.,0.));
#17517=DIRECTION('',(0.,1.,0.));
#17518=DIRECTION('center_axis',(0.,1.,0.));
#17519=DIRECTION('ref_axis',(1.,0.,0.));
#17520=DIRECTION('',(0.,1.,0.));
#17521=DIRECTION('center_axis',(-0.0913252028230577,0.,-0.99582112215464));
#17522=DIRECTION('ref_axis',(-0.99582112215464,0.,0.0913252028230577));
#17523=DIRECTION('',(0.,1.,0.));
#17524=DIRECTION('',(-0.99582112215464,0.,0.0913252028230577));
#17525=DIRECTION('center_axis',(-0.091325202823058,0.,0.99582112215464));
#17526=DIRECTION('ref_axis',(0.99582112215464,0.,0.091325202823058));
#17527=DIRECTION('',(0.99582112215464,0.,0.091325202823058));
#17528=DIRECTION('',(0.,1.,0.));
#17529=DIRECTION('center_axis',(0.,1.,0.));
#17530=DIRECTION('ref_axis',(-1.,0.,-1.22464679914735E-16));
#17531=DIRECTION('center_axis',(0.,1.,0.));
#17532=DIRECTION('ref_axis',(1.,0.,0.));
#17533=DIRECTION('center_axis',(0.,1.,0.));
#17534=DIRECTION('ref_axis',(1.,0.,0.));
#17535=DIRECTION('axis',(0.,0.,1.));
#17536=DIRECTION('refdir',(1.,0.,0.));
#17537=DIRECTION('center_axis',(0.,0.,1.));
#17538=DIRECTION('ref_axis',(1.,0.,0.));
#17539=DIRECTION('center_axis',(0.,0.,1.));
#17540=DIRECTION('ref_axis',(1.,0.,0.));
#17541=DIRECTION('',(0.,0.,1.));
#17542=DIRECTION('center_axis',(0.,0.,-1.));
#17543=DIRECTION('ref_axis',(1.,0.,0.));
#17544=DIRECTION('center_axis',(0.,0.,1.));
#17545=DIRECTION('ref_axis',(1.,0.,0.));
#17546=DIRECTION('center_axis',(0.,0.,1.));
#17547=DIRECTION('ref_axis',(1.,0.,0.));
#17548=DIRECTION('center_axis',(0.,0.,1.));
#17549=DIRECTION('ref_axis',(1.,0.,0.));
#17550=DIRECTION('center_axis',(0.,0.,1.));
#17551=DIRECTION('ref_axis',(1.,0.,0.));
#17552=DIRECTION('',(0.,0.,1.));
#17553=DIRECTION('center_axis',(0.,0.,1.));
#17554=DIRECTION('ref_axis',(1.,0.,0.));
#17555=DIRECTION('center_axis',(0.,0.,1.));
#17556=DIRECTION('ref_axis',(1.,0.,0.));
#17557=DIRECTION('',(0.,0.,1.));
#17558=DIRECTION('center_axis',(0.,0.,-1.));
#17559=DIRECTION('ref_axis',(1.,0.,0.));
#17560=DIRECTION('center_axis',(0.,0.,1.));
#17561=DIRECTION('ref_axis',(1.,0.,0.));
#17562=DIRECTION('center_axis',(0.,0.,1.));
#17563=DIRECTION('ref_axis',(1.,0.,0.));
#17564=DIRECTION('center_axis',(0.,0.,1.));
#17565=DIRECTION('ref_axis',(1.,0.,0.));
#17566=DIRECTION('center_axis',(0.,0.,1.));
#17567=DIRECTION('ref_axis',(1.,0.,0.));
#17568=DIRECTION('',(0.,0.,1.));
#17569=DIRECTION('center_axis',(0.,0.,1.));
#17570=DIRECTION('ref_axis',(1.,0.,0.));
#17571=DIRECTION('center_axis',(0.,0.,1.));
#17572=DIRECTION('ref_axis',(1.,0.,0.));
#17573=DIRECTION('',(0.,0.,1.));
#17574=DIRECTION('center_axis',(0.,0.,-1.));
#17575=DIRECTION('ref_axis',(1.,0.,0.));
#17576=DIRECTION('center_axis',(0.,0.,1.));
#17577=DIRECTION('ref_axis',(1.,0.,0.));
#17578=DIRECTION('center_axis',(0.,0.,1.));
#17579=DIRECTION('ref_axis',(1.,0.,0.));
#17580=DIRECTION('center_axis',(0.,0.,1.));
#17581=DIRECTION('ref_axis',(1.,0.,0.));
#17582=DIRECTION('center_axis',(0.,0.,1.));
#17583=DIRECTION('ref_axis',(1.,0.,0.));
#17584=DIRECTION('',(0.,0.,1.));
#17585=DIRECTION('center_axis',(0.,0.,1.));
#17586=DIRECTION('ref_axis',(1.,0.,0.));
#17587=DIRECTION('center_axis',(0.,0.,1.));
#17588=DIRECTION('ref_axis',(1.,0.,0.));
#17589=DIRECTION('',(0.,0.,1.));
#17590=DIRECTION('center_axis',(0.,0.,-1.));
#17591=DIRECTION('ref_axis',(1.,0.,0.));
#17592=DIRECTION('center_axis',(0.,0.,1.));
#17593=DIRECTION('ref_axis',(1.,0.,0.));
#17594=DIRECTION('center_axis',(0.,0.,1.));
#17595=DIRECTION('ref_axis',(1.,0.,0.));
#17596=DIRECTION('center_axis',(0.,0.,1.));
#17597=DIRECTION('ref_axis',(1.,0.,0.));
#17598=DIRECTION('center_axis',(0.,0.,1.));
#17599=DIRECTION('ref_axis',(1.,0.,0.));
#17600=DIRECTION('',(0.,0.,1.));
#17601=DIRECTION('center_axis',(0.,0.,1.));
#17602=DIRECTION('ref_axis',(1.,0.,0.));
#17603=DIRECTION('center_axis',(0.,0.,1.));
#17604=DIRECTION('ref_axis',(1.,0.,0.));
#17605=DIRECTION('',(0.,0.,1.));
#17606=DIRECTION('center_axis',(0.,0.,-1.));
#17607=DIRECTION('ref_axis',(1.,0.,0.));
#17608=DIRECTION('center_axis',(0.,0.,1.));
#17609=DIRECTION('ref_axis',(1.,0.,0.));
#17610=DIRECTION('center_axis',(0.,0.,1.));
#17611=DIRECTION('ref_axis',(1.,0.,0.));
#17612=DIRECTION('center_axis',(0.,0.,1.));
#17613=DIRECTION('ref_axis',(1.,0.,0.));
#17614=DIRECTION('',(0.,0.,1.));
#17615=DIRECTION('center_axis',(0.,0.,-1.));
#17616=DIRECTION('ref_axis',(1.,0.,0.));
#17617=DIRECTION('center_axis',(0.,0.,1.));
#17618=DIRECTION('ref_axis',(1.,0.,0.));
#17619=DIRECTION('center_axis',(0.,1.,0.));
#17620=DIRECTION('ref_axis',(-1.,0.,0.));
#17621=DIRECTION('',(-1.,0.,0.));
#17622=DIRECTION('',(0.,0.,1.));
#17623=DIRECTION('',(-1.,0.,0.));
#17624=DIRECTION('',(0.,0.,1.));
#17625=DIRECTION('center_axis',(1.,0.,0.));
#17626=DIRECTION('ref_axis',(0.,1.,0.));
#17627=DIRECTION('',(0.,1.,0.));
#17628=DIRECTION('',(0.,1.,0.));
#17629=DIRECTION('',(0.,0.,1.));
#17630=DIRECTION('center_axis',(0.,-1.,0.));
#17631=DIRECTION('ref_axis',(1.,0.,0.));
#17632=DIRECTION('',(1.,0.,0.));
#17633=DIRECTION('',(1.,0.,0.));
#17634=DIRECTION('',(0.,0.,1.));
#17635=DIRECTION('center_axis',(-1.,0.,0.));
#17636=DIRECTION('ref_axis',(0.,-1.,0.));
#17637=DIRECTION('',(0.,-1.,0.));
#17638=DIRECTION('',(0.,-1.,0.));
#17639=DIRECTION('center_axis',(0.,0.,1.));
#17640=DIRECTION('ref_axis',(1.,0.,0.));
#17641=DIRECTION('center_axis',(0.,0.,1.));
#17642=DIRECTION('ref_axis',(1.,0.,0.));
#17643=DIRECTION('axis',(0.,0.,1.));
#17644=DIRECTION('refdir',(1.,0.,0.));
#17645=DIRECTION('center_axis',(0.,0.,1.));
#17646=DIRECTION('ref_axis',(1.,0.,0.));
#17647=DIRECTION('center_axis',(0.,0.,-1.));
#17648=DIRECTION('ref_axis',(1.,0.,0.));
#17649=DIRECTION('',(0.,0.,-1.));
#17650=DIRECTION('center_axis',(0.,0.,-1.));
#17651=DIRECTION('ref_axis',(1.,0.,0.));
#17652=DIRECTION('center_axis',(0.,0.,1.));
#17653=DIRECTION('ref_axis',(1.,0.,0.));
#17654=DIRECTION('center_axis',(0.,0.,1.));
#17655=DIRECTION('ref_axis',(1.,0.,0.));
#17656=DIRECTION('',(0.,0.,-1.));
#17657=DIRECTION('center_axis',(0.,0.,1.));
#17658=DIRECTION('ref_axis',(1.,0.,0.));
#17659=DIRECTION('center_axis',(0.,0.,1.));
#17660=DIRECTION('ref_axis',(1.,0.,0.));
#17661=DIRECTION('center_axis',(0.,0.,1.));
#17662=DIRECTION('ref_axis',(1.,0.,0.));
#17663=DIRECTION('axis',(0.,0.,1.));
#17664=DIRECTION('refdir',(1.,0.,0.));
#17665=DIRECTION('center_axis',(0.,0.,1.));
#17666=DIRECTION('ref_axis',(1.,0.,0.));
#17667=DIRECTION('center_axis',(0.,0.,-1.));
#17668=DIRECTION('ref_axis',(1.,0.,0.));
#17669=DIRECTION('',(0.,0.,-1.));
#17670=DIRECTION('center_axis',(0.,0.,-1.));
#17671=DIRECTION('ref_axis',(1.,0.,0.));
#17672=DIRECTION('center_axis',(0.,0.,1.));
#17673=DIRECTION('ref_axis',(1.,0.,0.));
#17674=DIRECTION('center_axis',(0.,0.,1.));
#17675=DIRECTION('ref_axis',(1.,0.,0.));
#17676=DIRECTION('',(0.,0.,-1.));
#17677=DIRECTION('center_axis',(0.,0.,1.));
#17678=DIRECTION('ref_axis',(1.,0.,0.));
#17679=DIRECTION('center_axis',(0.,0.,1.));
#17680=DIRECTION('ref_axis',(1.,0.,0.));
#17681=DIRECTION('center_axis',(0.,0.,1.));
#17682=DIRECTION('ref_axis',(1.,0.,0.));
#17683=DIRECTION('axis',(0.,0.,1.));
#17684=DIRECTION('refdir',(1.,0.,0.));
#17685=DIRECTION('center_axis',(0.,0.,1.));
#17686=DIRECTION('ref_axis',(1.,0.,0.));
#17687=DIRECTION('center_axis',(0.,0.,1.));
#17688=DIRECTION('ref_axis',(1.,0.,0.));
#17689=DIRECTION('',(0.,0.,1.));
#17690=DIRECTION('center_axis',(0.,0.,-1.));
#17691=DIRECTION('ref_axis',(1.,0.,0.));
#17692=DIRECTION('center_axis',(0.,0.,1.));
#17693=DIRECTION('ref_axis',(1.,0.,0.));
#17694=DIRECTION('center_axis',(0.,0.,1.));
#17695=DIRECTION('ref_axis',(1.,0.,0.));
#17696=DIRECTION('center_axis',(0.,0.,1.));
#17697=DIRECTION('ref_axis',(1.,0.,0.));
#17698=DIRECTION('center_axis',(0.,0.,1.));
#17699=DIRECTION('ref_axis',(1.,0.,0.));
#17700=DIRECTION('',(0.,0.,1.));
#17701=DIRECTION('center_axis',(0.,0.,1.));
#17702=DIRECTION('ref_axis',(1.,0.,0.));
#17703=DIRECTION('center_axis',(0.,0.,1.));
#17704=DIRECTION('ref_axis',(1.,0.,0.));
#17705=DIRECTION('',(0.,0.,1.));
#17706=DIRECTION('center_axis',(0.,0.,-1.));
#17707=DIRECTION('ref_axis',(1.,0.,0.));
#17708=DIRECTION('center_axis',(0.,0.,1.));
#17709=DIRECTION('ref_axis',(1.,0.,0.));
#17710=DIRECTION('center_axis',(0.,0.,1.));
#17711=DIRECTION('ref_axis',(1.,0.,0.));
#17712=DIRECTION('center_axis',(0.,0.,1.));
#17713=DIRECTION('ref_axis',(1.,0.,0.));
#17714=DIRECTION('center_axis',(0.,0.,1.));
#17715=DIRECTION('ref_axis',(1.,0.,0.));
#17716=DIRECTION('',(0.,0.,1.));
#17717=DIRECTION('center_axis',(0.,0.,1.));
#17718=DIRECTION('ref_axis',(1.,0.,0.));
#17719=DIRECTION('center_axis',(0.,0.,1.));
#17720=DIRECTION('ref_axis',(1.,0.,0.));
#17721=DIRECTION('',(0.,0.,1.));
#17722=DIRECTION('center_axis',(0.,0.,-1.));
#17723=DIRECTION('ref_axis',(1.,0.,0.));
#17724=DIRECTION('center_axis',(0.,0.,1.));
#17725=DIRECTION('ref_axis',(1.,0.,0.));
#17726=DIRECTION('center_axis',(0.,0.,1.));
#17727=DIRECTION('ref_axis',(1.,0.,0.));
#17728=DIRECTION('center_axis',(0.,0.,1.));
#17729=DIRECTION('ref_axis',(1.,0.,0.));
#17730=DIRECTION('center_axis',(0.,0.,1.));
#17731=DIRECTION('ref_axis',(1.,0.,0.));
#17732=DIRECTION('',(0.,0.,1.));
#17733=DIRECTION('center_axis',(0.,0.,1.));
#17734=DIRECTION('ref_axis',(1.,0.,0.));
#17735=DIRECTION('center_axis',(0.,0.,1.));
#17736=DIRECTION('ref_axis',(1.,0.,0.));
#17737=DIRECTION('',(0.,0.,1.));
#17738=DIRECTION('center_axis',(0.,0.,-1.));
#17739=DIRECTION('ref_axis',(1.,0.,0.));
#17740=DIRECTION('center_axis',(0.,0.,1.));
#17741=DIRECTION('ref_axis',(1.,0.,0.));
#17742=DIRECTION('center_axis',(0.,0.,1.));
#17743=DIRECTION('ref_axis',(1.,0.,0.));
#17744=DIRECTION('center_axis',(0.,0.,1.));
#17745=DIRECTION('ref_axis',(1.,0.,0.));
#17746=DIRECTION('center_axis',(0.,0.,1.));
#17747=DIRECTION('ref_axis',(1.,0.,0.));
#17748=DIRECTION('',(0.,0.,1.));
#17749=DIRECTION('center_axis',(0.,0.,1.));
#17750=DIRECTION('ref_axis',(1.,0.,0.));
#17751=DIRECTION('center_axis',(0.,0.,1.));
#17752=DIRECTION('ref_axis',(1.,0.,0.));
#17753=DIRECTION('',(0.,0.,1.));
#17754=DIRECTION('center_axis',(0.,0.,-1.));
#17755=DIRECTION('ref_axis',(1.,0.,0.));
#17756=DIRECTION('center_axis',(0.,0.,1.));
#17757=DIRECTION('ref_axis',(1.,0.,0.));
#17758=DIRECTION('center_axis',(0.,0.,1.));
#17759=DIRECTION('ref_axis',(1.,0.,0.));
#17760=DIRECTION('center_axis',(0.,0.,1.));
#17761=DIRECTION('ref_axis',(1.,0.,0.));
#17762=DIRECTION('',(0.,0.,1.));
#17763=DIRECTION('center_axis',(0.,0.,-1.));
#17764=DIRECTION('ref_axis',(1.,0.,0.));
#17765=DIRECTION('center_axis',(0.,0.,1.));
#17766=DIRECTION('ref_axis',(1.,0.,0.));
#17767=DIRECTION('center_axis',(0.,1.,0.));
#17768=DIRECTION('ref_axis',(-1.,0.,0.));
#17769=DIRECTION('',(-1.,0.,0.));
#17770=DIRECTION('',(0.,0.,1.));
#17771=DIRECTION('',(-1.,0.,0.));
#17772=DIRECTION('',(0.,0.,1.));
#17773=DIRECTION('center_axis',(1.,0.,0.));
#17774=DIRECTION('ref_axis',(0.,1.,0.));
#17775=DIRECTION('',(0.,1.,0.));
#17776=DIRECTION('',(0.,1.,0.));
#17777=DIRECTION('',(0.,0.,1.));
#17778=DIRECTION('center_axis',(0.,-1.,0.));
#17779=DIRECTION('ref_axis',(1.,0.,0.));
#17780=DIRECTION('',(1.,0.,0.));
#17781=DIRECTION('',(1.,0.,0.));
#17782=DIRECTION('',(0.,0.,1.));
#17783=DIRECTION('center_axis',(-1.,0.,0.));
#17784=DIRECTION('ref_axis',(0.,-1.,0.));
#17785=DIRECTION('',(0.,-1.,0.));
#17786=DIRECTION('',(0.,-1.,0.));
#17787=DIRECTION('center_axis',(0.,0.,1.));
#17788=DIRECTION('ref_axis',(1.,0.,0.));
#17789=DIRECTION('center_axis',(0.,0.,1.));
#17790=DIRECTION('ref_axis',(1.,0.,0.));
#17791=DIRECTION('axis',(0.,0.,1.));
#17792=DIRECTION('refdir',(1.,0.,0.));
#17793=DIRECTION('center_axis',(0.,0.,1.));
#17794=DIRECTION('ref_axis',(1.,0.,0.));
#17795=DIRECTION('center_axis',(0.,0.,-1.));
#17796=DIRECTION('ref_axis',(1.,0.,0.));
#17797=DIRECTION('',(0.,0.,-1.));
#17798=DIRECTION('center_axis',(0.,0.,-1.));
#17799=DIRECTION('ref_axis',(1.,0.,0.));
#17800=DIRECTION('center_axis',(0.,0.,1.));
#17801=DIRECTION('ref_axis',(1.,0.,0.));
#17802=DIRECTION('center_axis',(0.,0.,1.));
#17803=DIRECTION('ref_axis',(1.,0.,0.));
#17804=DIRECTION('',(0.,0.,-1.));
#17805=DIRECTION('center_axis',(0.,0.,1.));
#17806=DIRECTION('ref_axis',(1.,0.,0.));
#17807=DIRECTION('center_axis',(0.,0.,1.));
#17808=DIRECTION('ref_axis',(1.,0.,0.));
#17809=DIRECTION('center_axis',(0.,0.,1.));
#17810=DIRECTION('ref_axis',(1.,0.,0.));
#17811=DIRECTION('axis',(0.,0.,1.));
#17812=DIRECTION('refdir',(1.,0.,0.));
#17813=DIRECTION('center_axis',(0.,0.,1.));
#17814=DIRECTION('ref_axis',(1.,0.,0.));
#17815=DIRECTION('center_axis',(0.,0.,-1.));
#17816=DIRECTION('ref_axis',(1.,0.,0.));
#17817=DIRECTION('',(0.,0.,-1.));
#17818=DIRECTION('center_axis',(0.,0.,-1.));
#17819=DIRECTION('ref_axis',(1.,0.,0.));
#17820=DIRECTION('center_axis',(0.,0.,1.));
#17821=DIRECTION('ref_axis',(1.,0.,0.));
#17822=DIRECTION('center_axis',(0.,0.,1.));
#17823=DIRECTION('ref_axis',(1.,0.,0.));
#17824=DIRECTION('',(0.,0.,-1.));
#17825=DIRECTION('center_axis',(0.,0.,1.));
#17826=DIRECTION('ref_axis',(1.,0.,0.));
#17827=DIRECTION('center_axis',(0.,0.,1.));
#17828=DIRECTION('ref_axis',(1.,0.,0.));
#17829=DIRECTION('center_axis',(0.,0.,1.));
#17830=DIRECTION('ref_axis',(1.,0.,0.));
#17831=DIRECTION('axis',(0.,0.,1.));
#17832=DIRECTION('refdir',(1.,0.,0.));
#17833=DIRECTION('center_axis',(0.,0.,1.));
#17834=DIRECTION('ref_axis',(1.,0.,0.));
#17835=DIRECTION('center_axis',(0.,0.,1.));
#17836=DIRECTION('ref_axis',(1.,0.,0.));
#17837=DIRECTION('',(0.,0.,1.));
#17838=DIRECTION('center_axis',(0.,0.,-1.));
#17839=DIRECTION('ref_axis',(1.,0.,0.));
#17840=DIRECTION('center_axis',(0.,0.,1.));
#17841=DIRECTION('ref_axis',(1.,0.,0.));
#17842=DIRECTION('center_axis',(0.,0.,1.));
#17843=DIRECTION('ref_axis',(1.,0.,0.));
#17844=DIRECTION('center_axis',(0.,0.,1.));
#17845=DIRECTION('ref_axis',(1.,0.,0.));
#17846=DIRECTION('center_axis',(0.,0.,1.));
#17847=DIRECTION('ref_axis',(1.,0.,0.));
#17848=DIRECTION('',(0.,0.,1.));
#17849=DIRECTION('center_axis',(0.,0.,1.));
#17850=DIRECTION('ref_axis',(1.,0.,0.));
#17851=DIRECTION('center_axis',(0.,0.,1.));
#17852=DIRECTION('ref_axis',(1.,0.,0.));
#17853=DIRECTION('',(0.,0.,1.));
#17854=DIRECTION('center_axis',(0.,0.,-1.));
#17855=DIRECTION('ref_axis',(1.,0.,0.));
#17856=DIRECTION('center_axis',(0.,0.,1.));
#17857=DIRECTION('ref_axis',(1.,0.,0.));
#17858=DIRECTION('center_axis',(0.,0.,1.));
#17859=DIRECTION('ref_axis',(1.,0.,0.));
#17860=DIRECTION('center_axis',(0.,0.,1.));
#17861=DIRECTION('ref_axis',(1.,0.,0.));
#17862=DIRECTION('center_axis',(0.,0.,1.));
#17863=DIRECTION('ref_axis',(1.,0.,0.));
#17864=DIRECTION('',(0.,0.,1.));
#17865=DIRECTION('center_axis',(0.,1.,0.));
#17866=DIRECTION('ref_axis',(-1.,0.,0.));
#17867=DIRECTION('',(-1.,0.,0.));
#17868=DIRECTION('',(0.,0.,1.));
#17869=DIRECTION('',(-1.,0.,0.));
#17870=DIRECTION('',(0.,0.,1.));
#17871=DIRECTION('center_axis',(1.,0.,0.));
#17872=DIRECTION('ref_axis',(0.,1.,0.));
#17873=DIRECTION('',(0.,1.,0.));
#17874=DIRECTION('',(0.,1.,0.));
#17875=DIRECTION('',(0.,0.,1.));
#17876=DIRECTION('center_axis',(0.,-1.,0.));
#17877=DIRECTION('ref_axis',(1.,0.,0.));
#17878=DIRECTION('',(1.,0.,0.));
#17879=DIRECTION('',(1.,0.,0.));
#17880=DIRECTION('',(0.,0.,1.));
#17881=DIRECTION('center_axis',(-1.,0.,0.));
#17882=DIRECTION('ref_axis',(0.,-1.,0.));
#17883=DIRECTION('',(0.,-1.,0.));
#17884=DIRECTION('',(0.,-1.,0.));
#17885=DIRECTION('center_axis',(0.,0.,1.));
#17886=DIRECTION('ref_axis',(1.,0.,0.));
#17887=DIRECTION('center_axis',(0.,0.,1.));
#17888=DIRECTION('ref_axis',(1.,0.,0.));
#17889=DIRECTION('axis',(0.,0.,1.));
#17890=DIRECTION('refdir',(1.,0.,0.));
#17891=DIRECTION('center_axis',(0.,1.,0.));
#17892=DIRECTION('ref_axis',(-1.,0.,0.));
#17893=DIRECTION('',(-1.,0.,0.));
#17894=DIRECTION('',(0.,0.,1.));
#17895=DIRECTION('',(-1.,0.,0.));
#17896=DIRECTION('',(0.,0.,1.));
#17897=DIRECTION('center_axis',(1.,0.,0.));
#17898=DIRECTION('ref_axis',(0.,1.,0.));
#17899=DIRECTION('',(0.,1.,0.));
#17900=DIRECTION('',(0.,1.,0.));
#17901=DIRECTION('',(0.,0.,1.));
#17902=DIRECTION('center_axis',(0.,-1.,0.));
#17903=DIRECTION('ref_axis',(1.,0.,0.));
#17904=DIRECTION('',(1.,0.,0.));
#17905=DIRECTION('',(1.,0.,0.));
#17906=DIRECTION('',(0.,0.,1.));
#17907=DIRECTION('center_axis',(-1.,0.,0.));
#17908=DIRECTION('ref_axis',(0.,-1.,0.));
#17909=DIRECTION('',(0.,-1.,0.));
#17910=DIRECTION('',(0.,-1.,0.));
#17911=DIRECTION('center_axis',(0.,0.,1.));
#17912=DIRECTION('ref_axis',(1.,0.,0.));
#17913=DIRECTION('center_axis',(0.,0.,1.));
#17914=DIRECTION('ref_axis',(1.,0.,0.));
#17915=DIRECTION('axis',(0.,0.,1.));
#17916=DIRECTION('refdir',(1.,0.,0.));
#17917=DIRECTION('center_axis',(0.,1.,0.));
#17918=DIRECTION('ref_axis',(1.,0.,0.));
#17919=DIRECTION('center_axis',(0.,1.,0.));
#17920=DIRECTION('ref_axis',(1.,0.,0.));
#17921=DIRECTION('',(0.,1.,0.));
#17922=DIRECTION('center_axis',(0.,-1.,0.));
#17923=DIRECTION('ref_axis',(1.,0.,0.));
#17924=DIRECTION('center_axis',(0.,1.,0.));
#17925=DIRECTION('ref_axis',(1.,0.,0.));
#17926=DIRECTION('center_axis',(0.,1.,0.));
#17927=DIRECTION('ref_axis',(1.,0.,0.));
#17928=DIRECTION('',(0.,1.,0.));
#17929=DIRECTION('center_axis',(0.,-1.,0.));
#17930=DIRECTION('ref_axis',(1.,0.,0.));
#17931=DIRECTION('center_axis',(0.,1.,0.));
#17932=DIRECTION('ref_axis',(-1.,0.,0.));
#17933=DIRECTION('',(-1.,0.,0.));
#17934=DIRECTION('',(0.,0.,1.));
#17935=DIRECTION('',(-1.,0.,0.));
#17936=DIRECTION('',(0.,0.,1.));
#17937=DIRECTION('center_axis',(1.,0.,0.));
#17938=DIRECTION('ref_axis',(0.,1.,0.));
#17939=DIRECTION('',(0.,1.,0.));
#17940=DIRECTION('',(0.,1.,0.));
#17941=DIRECTION('',(0.,0.,1.));
#17942=DIRECTION('center_axis',(0.,-1.,0.));
#17943=DIRECTION('ref_axis',(1.,0.,0.));
#17944=DIRECTION('',(1.,0.,0.));
#17945=DIRECTION('',(1.,0.,0.));
#17946=DIRECTION('',(0.,0.,1.));
#17947=DIRECTION('center_axis',(-1.,0.,0.));
#17948=DIRECTION('ref_axis',(0.,-1.,0.));
#17949=DIRECTION('',(0.,-1.,0.));
#17950=DIRECTION('',(0.,-1.,0.));
#17951=DIRECTION('center_axis',(0.,0.,1.));
#17952=DIRECTION('ref_axis',(1.,0.,0.));
#17953=DIRECTION('center_axis',(0.,0.,1.));
#17954=DIRECTION('ref_axis',(1.,0.,0.));
#17955=DIRECTION('axis',(0.,0.,1.));
#17956=DIRECTION('refdir',(1.,0.,0.));
#17957=DIRECTION('center_axis',(0.,1.,0.));
#17958=DIRECTION('ref_axis',(1.,0.,0.));
#17959=DIRECTION('center_axis',(0.,1.,0.));
#17960=DIRECTION('ref_axis',(1.,0.,0.));
#17961=DIRECTION('',(0.,1.,0.));
#17962=DIRECTION('center_axis',(0.,-1.,0.));
#17963=DIRECTION('ref_axis',(1.,0.,0.));
#17964=DIRECTION('center_axis',(0.,1.,0.));
#17965=DIRECTION('ref_axis',(1.,0.,0.));
#17966=DIRECTION('center_axis',(0.,1.,0.));
#17967=DIRECTION('ref_axis',(1.,0.,0.));
#17968=DIRECTION('',(0.,1.,0.));
#17969=DIRECTION('center_axis',(0.,-1.,0.));
#17970=DIRECTION('ref_axis',(1.,0.,0.));
#17971=DIRECTION('center_axis',(0.,1.,0.));
#17972=DIRECTION('ref_axis',(-1.,0.,0.));
#17973=DIRECTION('',(-1.,0.,0.));
#17974=DIRECTION('',(0.,0.,1.));
#17975=DIRECTION('',(-1.,0.,0.));
#17976=DIRECTION('',(0.,0.,1.));
#17977=DIRECTION('center_axis',(1.,0.,0.));
#17978=DIRECTION('ref_axis',(0.,1.,0.));
#17979=DIRECTION('',(0.,1.,0.));
#17980=DIRECTION('',(0.,1.,0.));
#17981=DIRECTION('',(0.,0.,1.));
#17982=DIRECTION('center_axis',(0.,-1.,0.));
#17983=DIRECTION('ref_axis',(1.,0.,0.));
#17984=DIRECTION('',(1.,0.,0.));
#17985=DIRECTION('',(1.,0.,0.));
#17986=DIRECTION('',(0.,0.,1.));
#17987=DIRECTION('center_axis',(-1.,0.,0.));
#17988=DIRECTION('ref_axis',(0.,-1.,0.));
#17989=DIRECTION('',(0.,-1.,0.));
#17990=DIRECTION('',(0.,-1.,0.));
#17991=DIRECTION('center_axis',(0.,0.,1.));
#17992=DIRECTION('ref_axis',(1.,0.,0.));
#17993=DIRECTION('center_axis',(0.,0.,1.));
#17994=DIRECTION('ref_axis',(1.,0.,0.));
#17995=DIRECTION('axis',(0.,0.,1.));
#17996=DIRECTION('refdir',(1.,0.,0.));
#17997=DIRECTION('center_axis',(0.,1.,0.));
#17998=DIRECTION('ref_axis',(1.,0.,0.));
#17999=DIRECTION('center_axis',(0.,1.,0.));
#18000=DIRECTION('ref_axis',(1.,0.,0.));
#18001=DIRECTION('',(0.,1.,0.));
#18002=DIRECTION('center_axis',(0.,-1.,0.));
#18003=DIRECTION('ref_axis',(1.,0.,0.));
#18004=DIRECTION('center_axis',(0.,1.,0.));
#18005=DIRECTION('ref_axis',(1.,0.,0.));
#18006=DIRECTION('center_axis',(0.,1.,0.));
#18007=DIRECTION('ref_axis',(1.,0.,0.));
#18008=DIRECTION('',(0.,1.,0.));
#18009=DIRECTION('center_axis',(0.,-1.,0.));
#18010=DIRECTION('ref_axis',(1.,0.,0.));
#18011=DIRECTION('center_axis',(0.,1.,0.));
#18012=DIRECTION('ref_axis',(1.,0.,0.));
#18013=DIRECTION('center_axis',(0.,1.,0.));
#18014=DIRECTION('ref_axis',(1.,0.,0.));
#18015=DIRECTION('',(0.,1.,0.));
#18016=DIRECTION('center_axis',(0.,-1.,0.));
#18017=DIRECTION('ref_axis',(1.,0.,0.));
#18018=DIRECTION('center_axis',(0.,1.,0.));
#18019=DIRECTION('ref_axis',(1.,0.,0.));
#18020=DIRECTION('center_axis',(0.,1.,0.));
#18021=DIRECTION('ref_axis',(1.,0.,0.));
#18022=DIRECTION('',(0.,1.,0.));
#18023=DIRECTION('center_axis',(0.,-1.,0.));
#18024=DIRECTION('ref_axis',(1.,0.,0.));
#18025=DIRECTION('center_axis',(-1.,0.,0.));
#18026=DIRECTION('ref_axis',(0.,0.,1.));
#18027=DIRECTION('',(0.,0.,-1.));
#18028=DIRECTION('',(0.,1.,0.));
#18029=DIRECTION('',(0.,0.,1.));
#18030=DIRECTION('',(0.,1.,0.));
#18031=DIRECTION('center_axis',(0.,0.,-1.));
#18032=DIRECTION('ref_axis',(-1.,0.,0.));
#18033=DIRECTION('',(1.,0.,0.));
#18034=DIRECTION('',(-1.,0.,0.));
#18035=DIRECTION('',(0.,1.,0.));
#18036=DIRECTION('center_axis',(1.,0.,0.));
#18037=DIRECTION('ref_axis',(0.,0.,-1.));
#18038=DIRECTION('',(0.,0.,1.));
#18039=DIRECTION('',(0.,0.,-1.));
#18040=DIRECTION('',(0.,1.,0.));
#18041=DIRECTION('center_axis',(0.,0.,1.));
#18042=DIRECTION('ref_axis',(1.,0.,0.));
#18043=DIRECTION('',(-1.,0.,0.));
#18044=DIRECTION('',(1.,0.,0.));
#18045=DIRECTION('center_axis',(0.,1.,0.));
#18046=DIRECTION('ref_axis',(0.,0.,1.));
#18047=DIRECTION('center_axis',(0.,1.,0.));
#18048=DIRECTION('ref_axis',(1.,0.,0.));
#18049=DIRECTION('axis',(0.,0.,1.));
#18050=DIRECTION('refdir',(1.,0.,0.));
#18051=DIRECTION('axis',(0.,0.,1.));
#18052=DIRECTION('refdir',(1.,0.,0.));
#18053=DIRECTION('center_axis',(0.,-1.,0.));
#18054=DIRECTION('ref_axis',(0.,0.,-1.));
#18055=DIRECTION('center_axis',(0.,-1.,0.));
#18056=DIRECTION('ref_axis',(1.,0.,0.));
#18057=DIRECTION('center_axis',(0.,-1.,0.));
#18058=DIRECTION('ref_axis',(1.,0.,0.));
#18059=DIRECTION('center_axis',(1.,0.,1.22464679914735E-16));
#18060=DIRECTION('ref_axis',(-1.22464679914735E-16,0.,1.));
#18061=DIRECTION('center_axis',(0.,1.,0.));
#18062=DIRECTION('ref_axis',(1.,0.,0.));
#18063=DIRECTION('center_axis',(0.,1.,0.));
#18064=DIRECTION('ref_axis',(1.,0.,0.));
#18065=DIRECTION('center_axis',(0.,-1.,0.));
#18066=DIRECTION('ref_axis',(1.,0.,0.));
#18067=DIRECTION('',(0.,1.,0.));
#18068=DIRECTION('center_axis',(0.,-1.,0.));
#18069=DIRECTION('ref_axis',(1.,0.,0.));
#18070=DIRECTION('center_axis',(0.,-1.,0.));
#18071=DIRECTION('ref_axis',(1.,0.,0.));
#18072=DIRECTION('center_axis',(0.,-1.,0.));
#18073=DIRECTION('ref_axis',(1.,0.,0.));
#18074=DIRECTION('',(0.,1.,0.));
#18075=DIRECTION('center_axis',(0.,-1.,0.));
#18076=DIRECTION('ref_axis',(1.,0.,0.));
#18077=DIRECTION('center_axis',(0.,1.,0.));
#18078=DIRECTION('ref_axis',(1.,0.,0.));
#18079=DIRECTION('',(-0.707106781186547,0.707106781186548,-8.65956056235493E-17));
#18080=DIRECTION('center_axis',(0.,-1.,0.));
#18081=DIRECTION('ref_axis',(1.,0.,0.));
#18082=DIRECTION('center_axis',(0.,1.,0.));
#18083=DIRECTION('ref_axis',(0.,0.,1.));
#18084=DIRECTION('center_axis',(0.,-1.,0.));
#18085=DIRECTION('ref_axis',(1.,0.,0.));
#18086=DIRECTION('center_axis',(0.,-1.,0.));
#18087=DIRECTION('ref_axis',(1.,0.,0.));
#18088=DIRECTION('',(0.,1.,0.));
#18089=DIRECTION('center_axis',(0.,-1.,0.));
#18090=DIRECTION('ref_axis',(0.,0.,-1.));
#18091=DIRECTION('center_axis',(0.,-1.,0.));
#18092=DIRECTION('ref_axis',(1.,0.,0.));
#18093=DIRECTION('center_axis',(0.,-1.,0.));
#18094=DIRECTION('ref_axis',(1.,0.,0.));
#18095=DIRECTION('',(0.707106781186547,0.707106781186548,8.65956056235493E-17));
#18096=DIRECTION('axis',(0.,0.,1.));
#18097=DIRECTION('refdir',(1.,0.,0.));
#18098=DIRECTION('center_axis',(0.,-1.,0.));
#18099=DIRECTION('ref_axis',(0.,0.,-1.));
#18100=DIRECTION('center_axis',(0.,-1.,0.));
#18101=DIRECTION('ref_axis',(1.,0.,0.));
#18102=DIRECTION('center_axis',(0.,-1.,0.));
#18103=DIRECTION('ref_axis',(1.,0.,0.));
#18104=DIRECTION('center_axis',(1.,0.,1.22464679914735E-16));
#18105=DIRECTION('ref_axis',(-1.22464679914735E-16,0.,1.));
#18106=DIRECTION('center_axis',(0.,1.,0.));
#18107=DIRECTION('ref_axis',(1.,0.,0.));
#18108=DIRECTION('center_axis',(0.,1.,0.));
#18109=DIRECTION('ref_axis',(1.,0.,0.));
#18110=DIRECTION('center_axis',(0.,-1.,0.));
#18111=DIRECTION('ref_axis',(1.,0.,0.));
#18112=DIRECTION('center_axis',(0.,-1.,0.));
#18113=DIRECTION('ref_axis',(1.,0.,0.));
#18114=DIRECTION('',(0.,1.,0.));
#18115=DIRECTION('center_axis',(0.,1.,0.));
#18116=DIRECTION('ref_axis',(0.,0.,1.));
#18117=DIRECTION('center_axis',(0.,-1.,0.));
#18118=DIRECTION('ref_axis',(1.,0.,0.));
#18119=DIRECTION('center_axis',(0.,-1.,0.));
#18120=DIRECTION('ref_axis',(1.,0.,0.));
#18121=DIRECTION('center_axis',(0.,-1.,0.));
#18122=DIRECTION('ref_axis',(1.,0.,0.));
#18123=DIRECTION('center_axis',(0.,-1.,0.));
#18124=DIRECTION('ref_axis',(1.,0.,0.));
#18125=DIRECTION('',(0.707106781186548,0.707106781186547,8.65956056235494E-17));
#18126=DIRECTION('center_axis',(0.,-1.,0.));
#18127=DIRECTION('ref_axis',(1.,0.,0.));
#18128=DIRECTION('center_axis',(0.,-1.,0.));
#18129=DIRECTION('ref_axis',(1.,0.,0.));
#18130=DIRECTION('',(0.,1.,0.));
#18131=DIRECTION('center_axis',(0.,1.,0.));
#18132=DIRECTION('ref_axis',(1.,0.,0.));
#18133=DIRECTION('center_axis',(0.,-1.,0.));
#18134=DIRECTION('ref_axis',(1.,0.,0.));
#18135=DIRECTION('',(-0.707106781186548,0.707106781186547,-8.65956056235494E-17));
#18136=DIRECTION('center_axis',(0.,-1.,0.));
#18137=DIRECTION('ref_axis',(0.,0.,-1.));
#18138=DIRECTION('center_axis',(0.,-1.,0.));
#18139=DIRECTION('ref_axis',(1.,0.,0.));
#18140=DIRECTION('',(0.,1.,0.));
#18141=DIRECTION('axis',(0.,0.,1.));
#18142=DIRECTION('refdir',(1.,0.,0.));
#18143=DIRECTION('center_axis',(0.,0.,1.));
#18144=DIRECTION('ref_axis',(1.,0.,0.));
#18145=DIRECTION('center_axis',(1.22464679914735E-16,-1.,0.));
#18146=DIRECTION('ref_axis',(-1.,-1.22464679914735E-16,0.));
#18147=DIRECTION('center_axis',(0.707106781186548,0.,0.707106781186548));
#18148=DIRECTION('ref_axis',(0.707106781186548,0.,-0.707106781186548));
#18149=DIRECTION('center_axis',(8.65956056235494E-17,-1.,-8.65956056235493E-17));
#18150=DIRECTION('ref_axis',(-0.707106781186547,-1.22464679914735E-16,0.707106781186547));
#18151=DIRECTION('center_axis',(1.,0.,0.));
#18152=DIRECTION('ref_axis',(6.12323399573676E-17,0.,-1.));
#18153=DIRECTION('center_axis',(7.49879891330929E-33,-1.,-1.22464679914735E-16));
#18154=DIRECTION('ref_axis',(-6.12323399573676E-17,-1.22464679914735E-16,
1.));
#18155=DIRECTION('center_axis',(0.707106781186548,0.,-0.707106781186548));
#18156=DIRECTION('ref_axis',(-0.707106781186548,0.,-0.707106781186548));
#18157=DIRECTION('center_axis',(-8.65956056235493E-17,-1.,-8.65956056235494E-17));
#18158=DIRECTION('ref_axis',(0.707106781186547,-1.22464679914735E-16,0.707106781186547));
#18159=DIRECTION('center_axis',(0.,0.,-1.));
#18160=DIRECTION('ref_axis',(-1.,0.,-1.22464679914735E-16));
#18161=DIRECTION('center_axis',(-1.22464679914735E-16,-1.,-1.49975978266186E-32));
#18162=DIRECTION('ref_axis',(1.,-1.22464679914735E-16,1.22464679914735E-16));
#18163=DIRECTION('center_axis',(-0.707106781186547,0.,-0.707106781186548));
#18164=DIRECTION('ref_axis',(-0.707106781186548,0.,0.707106781186547));
#18165=DIRECTION('center_axis',(-8.65956056235493E-17,-1.,8.65956056235493E-17));
#18166=DIRECTION('ref_axis',(0.707106781186548,-1.22464679914735E-16,-0.707106781186547));
#18167=DIRECTION('center_axis',(-1.,0.,0.));
#18168=DIRECTION('ref_axis',(-1.83697019872103E-16,0.,1.));
#18169=DIRECTION('center_axis',(-2.24963967399279E-32,-1.,1.22464679914735E-16));
#18170=DIRECTION('ref_axis',(1.83697019872103E-16,-1.22464679914735E-16,
-1.));
#18171=DIRECTION('center_axis',(-0.707106781186548,0.,0.707106781186548));
#18172=DIRECTION('ref_axis',(0.707106781186547,0.,0.707106781186548));
#18173=DIRECTION('center_axis',(8.65956056235493E-17,-1.,8.65956056235493E-17));
#18174=DIRECTION('ref_axis',(-0.707106781186547,-1.22464679914735E-16,-0.707106781186548));
#18175=DIRECTION('axis',(0.,0.,1.));
#18176=DIRECTION('refdir',(1.,0.,0.));
#18177=DIRECTION('center_axis',(0.,0.,1.));
#18178=DIRECTION('ref_axis',(1.,0.,0.));
#18179=DIRECTION('center_axis',(0.,-1.,0.));
#18180=DIRECTION('ref_axis',(0.,0.,-1.));
#18181=DIRECTION('center_axis',(0.,-1.,0.));
#18182=DIRECTION('ref_axis',(0.,0.,-1.));
#18183=DIRECTION('center_axis',(0.,1.,0.));
#18184=DIRECTION('ref_axis',(1.,0.,0.));
#18185=DIRECTION('center_axis',(0.,1.,0.));
#18186=DIRECTION('ref_axis',(1.,0.,0.));
#18187=DIRECTION('center_axis',(0.,1.,0.));
#18188=DIRECTION('ref_axis',(1.,0.,0.));
#18189=DIRECTION('center_axis',(0.,1.,0.));
#18190=DIRECTION('ref_axis',(1.,0.,0.));
#18191=DIRECTION('',(0.,-1.,0.));
#18192=DIRECTION('center_axis',(0.,-1.,0.));
#18193=DIRECTION('ref_axis',(1.,0.,0.));
#18194=DIRECTION('center_axis',(0.,1.,0.));
#18195=DIRECTION('ref_axis',(1.,0.,0.));
#18196=DIRECTION('center_axis',(0.,1.,0.));
#18197=DIRECTION('ref_axis',(1.,0.,0.));
#18198=DIRECTION('center_axis',(0.,1.,0.));
#18199=DIRECTION('ref_axis',(1.,0.,0.));
#18200=DIRECTION('center_axis',(0.,1.,0.));
#18201=DIRECTION('ref_axis',(1.,0.,0.));
#18202=DIRECTION('center_axis',(0.,1.,0.));
#18203=DIRECTION('ref_axis',(1.,0.,0.));
#18204=DIRECTION('center_axis',(0.,1.,0.));
#18205=DIRECTION('ref_axis',(1.,0.,0.));
#18206=DIRECTION('center_axis',(0.,-1.,0.));
#18207=DIRECTION('ref_axis',(1.,0.,0.));
#18208=DIRECTION('center_axis',(0.,-1.,0.));
#18209=DIRECTION('ref_axis',(0.,0.,-1.));
#18210=DIRECTION('center_axis',(6.12323399573677E-17,0.,1.));
#18211=DIRECTION('ref_axis',(1.,0.,0.));
#18212=DIRECTION('center_axis',(0.,-1.,0.));
#18213=DIRECTION('ref_axis',(0.,0.,-1.));
#18214=DIRECTION('center_axis',(0.,1.,0.));
#18215=DIRECTION('ref_axis',(1.,0.,0.));
#18216=DIRECTION('center_axis',(0.,-1.,0.));
#18217=DIRECTION('ref_axis',(1.,0.,0.));
#18218=DIRECTION('center_axis',(0.,-1.,0.));
#18219=DIRECTION('ref_axis',(0.,0.,-1.));
#18220=DIRECTION('center_axis',(0.,0.,1.));
#18221=DIRECTION('ref_axis',(1.,0.,0.));
#18222=DIRECTION('center_axis',(0.,-1.,0.));
#18223=DIRECTION('ref_axis',(0.,0.,-1.));
#18224=DIRECTION('center_axis',(0.,1.,0.));
#18225=DIRECTION('ref_axis',(1.,0.,0.));
#18226=DIRECTION('center_axis',(0.,-1.,0.));
#18227=DIRECTION('ref_axis',(1.,0.,0.));
#18228=DIRECTION('center_axis',(0.,-1.,0.));
#18229=DIRECTION('ref_axis',(0.,0.,-1.));
#18230=DIRECTION('center_axis',(0.,0.,1.));
#18231=DIRECTION('ref_axis',(1.,0.,0.));
#18232=DIRECTION('center_axis',(0.,-1.,0.));
#18233=DIRECTION('ref_axis',(0.,0.,-1.));
#18234=DIRECTION('center_axis',(0.,1.,0.));
#18235=DIRECTION('ref_axis',(1.,0.,0.));
#18236=DIRECTION('center_axis',(0.,-1.,0.));
#18237=DIRECTION('ref_axis',(1.,0.,0.));
#18238=DIRECTION('center_axis',(0.,-1.,0.));
#18239=DIRECTION('ref_axis',(0.,0.,-1.));
#18240=DIRECTION('center_axis',(0.,0.,1.));
#18241=DIRECTION('ref_axis',(1.,0.,0.));
#18242=DIRECTION('center_axis',(0.,-1.,0.));
#18243=DIRECTION('ref_axis',(0.,0.,-1.));
#18244=DIRECTION('center_axis',(0.,1.,0.));
#18245=DIRECTION('ref_axis',(1.,0.,0.));
#18246=DIRECTION('center_axis',(0.,-1.,0.));
#18247=DIRECTION('ref_axis',(1.,0.,0.));
#18248=DIRECTION('center_axis',(0.,-1.,0.));
#18249=DIRECTION('ref_axis',(0.,0.,-1.));
#18250=DIRECTION('center_axis',(6.12323399573676E-17,0.,1.));
#18251=DIRECTION('ref_axis',(1.,0.,0.));
#18252=DIRECTION('center_axis',(0.,-1.,0.));
#18253=DIRECTION('ref_axis',(0.,0.,-1.));
#18254=DIRECTION('center_axis',(0.,1.,0.));
#18255=DIRECTION('ref_axis',(1.,0.,0.));
#18256=DIRECTION('center_axis',(0.,-1.,0.));
#18257=DIRECTION('ref_axis',(1.,0.,0.));
#18258=DIRECTION('center_axis',(0.,-1.,0.));
#18259=DIRECTION('ref_axis',(0.,0.,-1.));
#18260=DIRECTION('center_axis',(0.,0.,1.));
#18261=DIRECTION('ref_axis',(1.,0.,0.));
#18262=DIRECTION('center_axis',(0.,-1.,0.));
#18263=DIRECTION('ref_axis',(0.,0.,-1.));
#18264=DIRECTION('center_axis',(0.,1.,0.));
#18265=DIRECTION('ref_axis',(1.,0.,0.));
#18266=DIRECTION('center_axis',(0.,1.,0.));
#18267=DIRECTION('ref_axis',(1.,0.,0.));
#18268=DIRECTION('',(0.,1.,0.));
#18269=DIRECTION('center_axis',(0.,-1.,0.));
#18270=DIRECTION('ref_axis',(1.,0.,0.));
#18271=DIRECTION('center_axis',(0.,-1.,0.));
#18272=DIRECTION('ref_axis',(1.,0.,0.));
#18273=DIRECTION('center_axis',(0.,1.,0.));
#18274=DIRECTION('ref_axis',(1.,0.,0.));
#18275=DIRECTION('center_axis',(0.,-1.,0.));
#18276=DIRECTION('ref_axis',(0.,0.,-1.));
#18277=DIRECTION('center_axis',(0.,0.,1.));
#18278=DIRECTION('ref_axis',(1.,0.,0.));
#18279=DIRECTION('center_axis',(0.,-1.,0.));
#18280=DIRECTION('ref_axis',(0.,0.,-1.));
#18281=DIRECTION('center_axis',(0.,-1.,0.));
#18282=DIRECTION('ref_axis',(-1.,0.,0.));
#18283=DIRECTION('center_axis',(0.,1.,0.));
#18284=DIRECTION('ref_axis',(1.,0.,0.));
#18285=DIRECTION('axis',(0.,0.,1.));
#18286=DIRECTION('refdir',(1.,0.,0.));
#18287=DIRECTION('center_axis',(0.,1.,0.));
#18288=DIRECTION('ref_axis',(0.,0.,1.));
#18289=DIRECTION('center_axis',(0.,-1.,0.));
#18290=DIRECTION('ref_axis',(1.,0.,0.));
#18291=DIRECTION('center_axis',(0.,-1.,0.));
#18292=DIRECTION('ref_axis',(1.,0.,0.));
#18293=DIRECTION('center_axis',(0.,-1.,0.));
#18294=DIRECTION('ref_axis',(1.,0.,0.));
#18295=DIRECTION('center_axis',(0.,-1.,0.));
#18296=DIRECTION('ref_axis',(1.,0.,0.));
#18297=DIRECTION('',(0.,1.,0.));
#18298=DIRECTION('center_axis',(0.,-1.,0.));
#18299=DIRECTION('ref_axis',(0.,0.,-1.));
#18300=DIRECTION('center_axis',(0.,-1.,0.));
#18301=DIRECTION('ref_axis',(1.,0.,0.));
#18302=DIRECTION('center_axis',(0.,-1.,0.));
#18303=DIRECTION('ref_axis',(1.,0.,0.));
#18304=DIRECTION('',(0.,1.,0.));
#18305=DIRECTION('center_axis',(0.,1.,0.));
#18306=DIRECTION('ref_axis',(0.,0.,1.));
#18307=DIRECTION('center_axis',(0.,-1.,0.));
#18308=DIRECTION('ref_axis',(1.,0.,0.));
#18309=DIRECTION('center_axis',(0.,-1.,0.));
#18310=DIRECTION('ref_axis',(1.,0.,0.));
#18311=DIRECTION('center_axis',(0.,-1.,0.));
#18312=DIRECTION('ref_axis',(1.,0.,0.));
#18313=DIRECTION('center_axis',(0.,-1.,0.));
#18314=DIRECTION('ref_axis',(1.,0.,0.));
#18315=DIRECTION('',(0.,1.,0.));
#18316=DIRECTION('center_axis',(0.,-1.,0.));
#18317=DIRECTION('ref_axis',(0.,0.,-1.));
#18318=DIRECTION('center_axis',(0.,-1.,0.));
#18319=DIRECTION('ref_axis',(1.,0.,0.));
#18320=DIRECTION('center_axis',(0.,-1.,0.));
#18321=DIRECTION('ref_axis',(1.,0.,0.));
#18322=DIRECTION('',(0.,1.,0.));
#18323=DIRECTION('',(0.,0.,1.));
#18324=DIRECTION('',(1.,0.,0.));
#18325=DIRECTION('',(0.,0.,1.));
#18326=DIRECTION('',(1.,0.,0.));
#18327=DIRECTION('',(0.,0.,1.));
#18328=DIRECTION('',(1.,0.,0.));
#18329=DIRECTION('',(0.,0.,1.));
#18330=DIRECTION('',(1.,0.,0.));
#18331=DIRECTION('',(0.,0.,1.));
#18332=DIRECTION('',(1.,0.,0.));
#18333=DIRECTION('axis',(0.,0.,1.));
#18334=DIRECTION('refdir',(1.,0.,0.));
#18335=DIRECTION('center_axis',(0.866025403784439,0.,-0.5));
#18336=DIRECTION('ref_axis',(0.5,0.,0.866025403784439));
#18337=DIRECTION('',(-0.5,0.,-0.866025403784439));
#18338=DIRECTION('',(0.,-1.,0.));
#18339=DIRECTION('',(0.5,0.,0.866025403784439));
#18340=DIRECTION('',(0.,-1.,0.));
#18341=DIRECTION('center_axis',(1.60246890531964E-16,0.,-1.));
#18342=DIRECTION('ref_axis',(1.,0.,1.60246890531964E-16));
#18343=DIRECTION('',(-1.,0.,-1.60246890531964E-16));
#18344=DIRECTION('',(0.,-1.,0.));
#18345=DIRECTION('',(1.,0.,1.60246890531964E-16));
#18346=DIRECTION('center_axis',(-0.866025403784439,0.,-0.5));
#18347=DIRECTION('ref_axis',(0.5,0.,-0.866025403784439));
#18348=DIRECTION('',(-0.5,0.,0.866025403784439));
#18349=DIRECTION('',(0.,-1.,0.));
#18350=DIRECTION('',(0.5,0.,-0.866025403784439));
#18351=DIRECTION('center_axis',(-0.866025403784439,0.,0.5));
#18352=DIRECTION('ref_axis',(-0.5,0.,-0.866025403784439));
#18353=DIRECTION('',(0.5,0.,0.866025403784439));
#18354=DIRECTION('',(0.,-1.,0.));
#18355=DIRECTION('',(-0.5,0.,-0.866025403784439));
#18356=DIRECTION('center_axis',(-1.60246890531964E-16,0.,1.));
#18357=DIRECTION('ref_axis',(-1.,0.,-1.60246890531964E-16));
#18358=DIRECTION('',(1.,0.,1.60246890531964E-16));
#18359=DIRECTION('',(0.,-1.,0.));
#18360=DIRECTION('',(-1.,0.,-1.60246890531964E-16));
#18361=DIRECTION('center_axis',(0.866025403784439,0.,0.5));
#18362=DIRECTION('ref_axis',(-0.5,0.,0.866025403784439));
#18363=DIRECTION('',(0.5,0.,-0.866025403784439));
#18364=DIRECTION('',(-0.5,0.,0.866025403784439));
#18365=DIRECTION('center_axis',(0.,1.,0.));
#18366=DIRECTION('ref_axis',(1.,0.,0.));
#18367=DIRECTION('center_axis',(0.,-1.,0.));
#18368=DIRECTION('ref_axis',(0.,0.,-1.));
#18369=DIRECTION('center_axis',(0.,1.,0.));
#18370=DIRECTION('ref_axis',(1.,0.,0.));
#18371=DIRECTION('center_axis',(0.,1.,0.));
#18372=DIRECTION('ref_axis',(1.,0.,0.));
#18373=DIRECTION('center_axis',(0.,-1.,0.));
#18374=DIRECTION('ref_axis',(1.,0.,0.));
#18375=DIRECTION('center_axis',(0.,1.,0.));
#18376=DIRECTION('ref_axis',(1.,0.,0.));
#18377=DIRECTION('',(0.,-1.,0.));
#18378=DIRECTION('center_axis',(0.,1.,0.));
#18379=DIRECTION('ref_axis',(1.,0.,0.));
#18380=DIRECTION('center_axis',(0.,1.,0.));
#18381=DIRECTION('ref_axis',(1.,0.,0.));
#18382=DIRECTION('center_axis',(0.,1.,0.));
#18383=DIRECTION('ref_axis',(0.,0.,1.));
#18384=DIRECTION('center_axis',(0.,-1.,0.));
#18385=DIRECTION('ref_axis',(1.,0.,0.));
#18386=DIRECTION('center_axis',(0.,-1.,0.));
#18387=DIRECTION('ref_axis',(1.,0.,0.));
#18388=DIRECTION('center_axis',(0.,-1.,0.));
#18389=DIRECTION('ref_axis',(1.,0.,0.));
#18390=DIRECTION('',(0.707106781186547,0.707106781186548,8.65956056235493E-17));
#18391=DIRECTION('center_axis',(0.,-1.,0.));
#18392=DIRECTION('ref_axis',(1.,0.,0.));
#18393=DIRECTION('center_axis',(0.,-1.,0.));
#18394=DIRECTION('ref_axis',(1.,0.,0.));
#18395=DIRECTION('',(0.,1.,0.));
#18396=DIRECTION('center_axis',(0.,1.,0.));
#18397=DIRECTION('ref_axis',(1.,0.,0.));
#18398=DIRECTION('center_axis',(0.,-1.,0.));
#18399=DIRECTION('ref_axis',(1.,0.,0.));
#18400=DIRECTION('',(-0.707106781186547,0.707106781186548,-8.65956056235493E-17));
#18401=DIRECTION('center_axis',(0.,-1.,0.));
#18402=DIRECTION('ref_axis',(0.,0.,-1.));
#18403=DIRECTION('center_axis',(0.,-1.,0.));
#18404=DIRECTION('ref_axis',(1.,0.,0.));
#18405=DIRECTION('center_axis',(0.,1.,0.));
#18406=DIRECTION('ref_axis',(1.,0.,0.));
#18407=DIRECTION('center_axis',(0.,1.,0.));
#18408=DIRECTION('ref_axis',(1.,0.,0.));
#18409=DIRECTION('',(-0.447213595499958,0.894427190999916,-5.47678698264203E-17));
#18410=DIRECTION('center_axis',(0.,-1.,0.));
#18411=DIRECTION('ref_axis',(1.,0.,0.));
#18412=DIRECTION('center_axis',(0.,1.,0.));
#18413=DIRECTION('ref_axis',(1.,0.,0.));
#18414=DIRECTION('',(0.,1.,0.));
#18415=DIRECTION('center_axis',(0.,1.,0.));
#18416=DIRECTION('ref_axis',(1.,0.,0.));
#18417=DIRECTION('',(-0.707106781186547,0.707106781186548,-8.65956056235493E-17));
#18418=DIRECTION('axis',(0.,0.,1.));
#18419=DIRECTION('refdir',(1.,0.,0.));
#18420=DIRECTION('axis',(0.,0.,1.));
#18421=DIRECTION('refdir',(1.,0.,0.));
#18422=DIRECTION('center_axis',(0.,-1.,0.));
#18423=DIRECTION('ref_axis',(0.,0.,-1.));
#18424=DIRECTION('center_axis',(0.,-1.,0.));
#18425=DIRECTION('ref_axis',(1.,0.,0.));
#18426=DIRECTION('center_axis',(0.,-1.,0.));
#18427=DIRECTION('ref_axis',(1.,0.,0.));
#18428=DIRECTION('center_axis',(1.,0.,1.22464679914735E-16));
#18429=DIRECTION('ref_axis',(-1.22464679914735E-16,0.,1.));
#18430=DIRECTION('center_axis',(0.,1.,0.));
#18431=DIRECTION('ref_axis',(1.,0.,0.));
#18432=DIRECTION('center_axis',(0.,1.,0.));
#18433=DIRECTION('ref_axis',(1.,0.,0.));
#18434=DIRECTION('center_axis',(0.,-1.,0.));
#18435=DIRECTION('ref_axis',(1.,0.,0.));
#18436=DIRECTION('',(0.,1.,0.));
#18437=DIRECTION('center_axis',(0.,-1.,0.));
#18438=DIRECTION('ref_axis',(1.,0.,0.));
#18439=DIRECTION('center_axis',(0.,-1.,0.));
#18440=DIRECTION('ref_axis',(1.,0.,0.));
#18441=DIRECTION('center_axis',(0.,-1.,0.));
#18442=DIRECTION('ref_axis',(1.,0.,0.));
#18443=DIRECTION('',(0.,1.,0.));
#18444=DIRECTION('center_axis',(0.,-1.,0.));
#18445=DIRECTION('ref_axis',(1.,0.,0.));
#18446=DIRECTION('center_axis',(0.,1.,0.));
#18447=DIRECTION('ref_axis',(1.,0.,0.));
#18448=DIRECTION('',(-0.707106781186548,0.707106781186547,-8.65956056235493E-17));
#18449=DIRECTION('center_axis',(0.,-1.,0.));
#18450=DIRECTION('ref_axis',(1.,0.,0.));
#18451=DIRECTION('center_axis',(0.,1.,0.));
#18452=DIRECTION('ref_axis',(0.,0.,1.));
#18453=DIRECTION('center_axis',(0.,-1.,0.));
#18454=DIRECTION('ref_axis',(1.,0.,0.));
#18455=DIRECTION('center_axis',(0.,-1.,0.));
#18456=DIRECTION('ref_axis',(1.,0.,0.));
#18457=DIRECTION('',(0.,1.,0.));
#18458=DIRECTION('center_axis',(0.,-1.,0.));
#18459=DIRECTION('ref_axis',(0.,0.,-1.));
#18460=DIRECTION('center_axis',(0.,-1.,0.));
#18461=DIRECTION('ref_axis',(1.,0.,0.));
#18462=DIRECTION('center_axis',(0.,-1.,0.));
#18463=DIRECTION('ref_axis',(1.,0.,0.));
#18464=DIRECTION('',(0.707106781186548,0.707106781186547,8.65956056235493E-17));
#18465=DIRECTION('axis',(0.,0.,1.));
#18466=DIRECTION('refdir',(1.,0.,0.));
#18467=DIRECTION('center_axis',(0.,-1.,0.));
#18468=DIRECTION('ref_axis',(0.,0.,-1.));
#18469=DIRECTION('center_axis',(0.,-1.,0.));
#18470=DIRECTION('ref_axis',(1.,0.,0.));
#18471=DIRECTION('center_axis',(0.,-1.,0.));
#18472=DIRECTION('ref_axis',(1.,0.,0.));
#18473=DIRECTION('center_axis',(1.,0.,1.22464679914735E-16));
#18474=DIRECTION('ref_axis',(-1.22464679914735E-16,0.,1.));
#18475=DIRECTION('center_axis',(0.,1.,0.));
#18476=DIRECTION('ref_axis',(1.,0.,0.));
#18477=DIRECTION('center_axis',(0.,1.,0.));
#18478=DIRECTION('ref_axis',(1.,0.,0.));
#18479=DIRECTION('center_axis',(0.,-1.,0.));
#18480=DIRECTION('ref_axis',(1.,0.,0.));
#18481=DIRECTION('center_axis',(0.,-1.,0.));
#18482=DIRECTION('ref_axis',(1.,0.,0.));
#18483=DIRECTION('',(0.,1.,0.));
#18484=DIRECTION('center_axis',(0.,1.,0.));
#18485=DIRECTION('ref_axis',(0.,0.,1.));
#18486=DIRECTION('center_axis',(0.,-1.,0.));
#18487=DIRECTION('ref_axis',(1.,0.,0.));
#18488=DIRECTION('center_axis',(0.,-1.,0.));
#18489=DIRECTION('ref_axis',(1.,0.,0.));
#18490=DIRECTION('center_axis',(0.,-1.,0.));
#18491=DIRECTION('ref_axis',(1.,0.,0.));
#18492=DIRECTION('center_axis',(0.,-1.,0.));
#18493=DIRECTION('ref_axis',(1.,0.,0.));
#18494=DIRECTION('',(0.707106781186548,0.707106781186547,8.65956056235494E-17));
#18495=DIRECTION('center_axis',(0.,-1.,0.));
#18496=DIRECTION('ref_axis',(1.,0.,0.));
#18497=DIRECTION('center_axis',(0.,-1.,0.));
#18498=DIRECTION('ref_axis',(1.,0.,0.));
#18499=DIRECTION('',(0.,1.,0.));
#18500=DIRECTION('center_axis',(0.,1.,0.));
#18501=DIRECTION('ref_axis',(1.,0.,0.));
#18502=DIRECTION('center_axis',(0.,-1.,0.));
#18503=DIRECTION('ref_axis',(1.,0.,0.));
#18504=DIRECTION('',(-0.707106781186548,0.707106781186547,-8.65956056235494E-17));
#18505=DIRECTION('center_axis',(0.,-1.,0.));
#18506=DIRECTION('ref_axis',(0.,0.,-1.));
#18507=DIRECTION('center_axis',(0.,-1.,0.));
#18508=DIRECTION('ref_axis',(1.,0.,0.));
#18509=DIRECTION('',(0.,1.,0.));
#18510=DIRECTION('axis',(0.,0.,1.));
#18511=DIRECTION('refdir',(1.,0.,0.));
#18512=DIRECTION('center_axis',(0.,0.,1.));
#18513=DIRECTION('ref_axis',(1.,0.,0.));
#18514=DIRECTION('center_axis',(1.22464679914735E-16,-1.,0.));
#18515=DIRECTION('ref_axis',(-1.,-1.22464679914735E-16,0.));
#18516=DIRECTION('center_axis',(0.78183148246803,0.,0.623489801858733));
#18517=DIRECTION('ref_axis',(0.623489801858734,0.,-0.78183148246803));
#18518=DIRECTION('center_axis',(7.63554790147315E-17,-1.,-9.57467422477103E-17));
#18519=DIRECTION('ref_axis',(-0.623489801858734,-1.22464679914735E-16,0.78183148246803));
#18520=DIRECTION('center_axis',(0.974927912181824,0.,-0.222520933956314));
#18521=DIRECTION('ref_axis',(-0.222520933956314,0.,-0.974927912181824));
#18522=DIRECTION('center_axis',(-2.7250954951288E-17,-1.,-1.19394234705288E-16));
#18523=DIRECTION('ref_axis',(0.222520933956314,-1.22464679914735E-16,0.974927912181824));
#18524=DIRECTION('center_axis',(0.433883739117558,0.,-0.900968867902419));
#18525=DIRECTION('ref_axis',(-0.900968867902419,0.,-0.433883739117558));
#18526=DIRECTION('center_axis',(-1.10336864020811E-16,-1.,-5.31354332312403E-17));
#18527=DIRECTION('ref_axis',(0.900968867902419,-1.22464679914735E-16,0.433883739117558));
#18528=DIRECTION('center_axis',(-0.433883739117558,0.,-0.900968867902419));
#18529=DIRECTION('ref_axis',(-0.900968867902419,0.,0.433883739117558));
#18530=DIRECTION('center_axis',(-1.10336864020811E-16,-1.,5.31354332312403E-17));
#18531=DIRECTION('ref_axis',(0.900968867902419,-1.22464679914735E-16,-0.433883739117558));
#18532=DIRECTION('center_axis',(-0.974927912181824,0.,-0.222520933956314));
#18533=DIRECTION('ref_axis',(-0.222520933956315,0.,0.974927912181824));
#18534=DIRECTION('center_axis',(-2.7250954951288E-17,-1.,1.19394234705288E-16));
#18535=DIRECTION('ref_axis',(0.222520933956315,-1.22464679914735E-16,-0.974927912181824));
#18536=DIRECTION('center_axis',(-0.78183148246803,0.,0.623489801858734));
#18537=DIRECTION('ref_axis',(0.623489801858733,0.,0.78183148246803));
#18538=DIRECTION('center_axis',(7.63554790147315E-17,-1.,9.57467422477103E-17));
#18539=DIRECTION('ref_axis',(-0.623489801858733,-1.22464679914735E-16,-0.78183148246803));
#18540=DIRECTION('axis',(0.,0.,1.));
#18541=DIRECTION('refdir',(1.,0.,0.));
#18542=DIRECTION('center_axis',(0.,0.,1.));
#18543=DIRECTION('ref_axis',(1.,0.,0.));
#18544=DIRECTION('center_axis',(0.,-1.,0.));
#18545=DIRECTION('ref_axis',(0.,0.,-1.));
#18546=DIRECTION('center_axis',(0.,-1.,0.));
#18547=DIRECTION('ref_axis',(0.,0.,-1.));
#18548=DIRECTION('center_axis',(0.,1.,0.));
#18549=DIRECTION('ref_axis',(1.,0.,0.));
#18550=DIRECTION('center_axis',(0.,1.,0.));
#18551=DIRECTION('ref_axis',(1.,0.,0.));
#18552=DIRECTION('center_axis',(0.,1.,0.));
#18553=DIRECTION('ref_axis',(1.,0.,0.));
#18554=DIRECTION('center_axis',(0.,1.,0.));
#18555=DIRECTION('ref_axis',(1.,0.,0.));
#18556=DIRECTION('',(0.,-1.,0.));
#18557=DIRECTION('center_axis',(0.,-1.,0.));
#18558=DIRECTION('ref_axis',(1.,0.,0.));
#18559=DIRECTION('center_axis',(0.,1.,0.));
#18560=DIRECTION('ref_axis',(1.,0.,0.));
#18561=DIRECTION('center_axis',(0.,1.,0.));
#18562=DIRECTION('ref_axis',(1.,0.,0.));
#18563=DIRECTION('center_axis',(0.,1.,0.));
#18564=DIRECTION('ref_axis',(1.,0.,0.));
#18565=DIRECTION('center_axis',(0.,1.,0.));
#18566=DIRECTION('ref_axis',(1.,0.,0.));
#18567=DIRECTION('center_axis',(0.,1.,0.));
#18568=DIRECTION('ref_axis',(1.,0.,0.));
#18569=DIRECTION('center_axis',(0.,1.,0.));
#18570=DIRECTION('ref_axis',(1.,0.,0.));
#18571=DIRECTION('center_axis',(0.,-1.,0.));
#18572=DIRECTION('ref_axis',(1.,0.,0.));
#18573=DIRECTION('center_axis',(0.,-1.,0.));
#18574=DIRECTION('ref_axis',(0.,0.,-1.));
#18575=DIRECTION('center_axis',(8.96625347776458E-17,0.,1.));
#18576=DIRECTION('ref_axis',(1.,0.,0.));
#18577=DIRECTION('center_axis',(0.,-1.,0.));
#18578=DIRECTION('ref_axis',(0.,0.,-1.));
#18579=DIRECTION('center_axis',(0.,1.,0.));
#18580=DIRECTION('ref_axis',(1.,0.,0.));
#18581=DIRECTION('center_axis',(0.,-1.,0.));
#18582=DIRECTION('ref_axis',(1.,0.,0.));
#18583=DIRECTION('center_axis',(0.,-1.,0.));
#18584=DIRECTION('ref_axis',(0.,0.,-1.));
#18585=DIRECTION('center_axis',(0.,0.,1.));
#18586=DIRECTION('ref_axis',(1.,0.,0.));
#18587=DIRECTION('center_axis',(0.,-1.,0.));
#18588=DIRECTION('ref_axis',(0.,0.,-1.));
#18589=DIRECTION('center_axis',(0.,1.,0.));
#18590=DIRECTION('ref_axis',(1.,0.,0.));
#18591=DIRECTION('center_axis',(0.,-1.,0.));
#18592=DIRECTION('ref_axis',(1.,0.,0.));
#18593=DIRECTION('center_axis',(0.,-1.,0.));
#18594=DIRECTION('ref_axis',(1.,0.,0.));
#18595=DIRECTION('center_axis',(0.,-1.,0.));
#18596=DIRECTION('ref_axis',(0.,0.,-1.));
#18597=DIRECTION('center_axis',(0.,0.,1.));
#18598=DIRECTION('ref_axis',(1.,0.,0.));
#18599=DIRECTION('center_axis',(0.,-1.,0.));
#18600=DIRECTION('ref_axis',(0.,0.,-1.));
#18601=DIRECTION('center_axis',(0.,1.,0.));
#18602=DIRECTION('ref_axis',(1.,0.,0.));
#18603=DIRECTION('center_axis',(0.,-1.,0.));
#18604=DIRECTION('ref_axis',(1.,0.,0.));
#18605=DIRECTION('center_axis',(0.,-1.,0.));
#18606=DIRECTION('ref_axis',(0.,0.,-1.));
#18607=DIRECTION('center_axis',(8.96625347776458E-17,0.,1.));
#18608=DIRECTION('ref_axis',(1.,0.,0.));
#18609=DIRECTION('center_axis',(0.,-1.,0.));
#18610=DIRECTION('ref_axis',(0.,0.,-1.));
#18611=DIRECTION('center_axis',(0.,1.,0.));
#18612=DIRECTION('ref_axis',(1.,0.,0.));
#18613=DIRECTION('center_axis',(0.,-1.,0.));
#18614=DIRECTION('ref_axis',(1.,0.,0.));
#18615=DIRECTION('center_axis',(0.,-1.,0.));
#18616=DIRECTION('ref_axis',(0.,0.,-1.));
#18617=DIRECTION('center_axis',(0.,0.,1.));
#18618=DIRECTION('ref_axis',(1.,0.,0.));
#18619=DIRECTION('center_axis',(0.,-1.,0.));
#18620=DIRECTION('ref_axis',(0.,0.,-1.));
#18621=DIRECTION('center_axis',(0.,1.,0.));
#18622=DIRECTION('ref_axis',(1.,0.,0.));
#18623=DIRECTION('center_axis',(0.,1.,0.));
#18624=DIRECTION('ref_axis',(1.,0.,0.));
#18625=DIRECTION('',(0.,1.,0.));
#18626=DIRECTION('center_axis',(0.,-1.,0.));
#18627=DIRECTION('ref_axis',(1.,0.,0.));
#18628=DIRECTION('center_axis',(0.,-1.,0.));
#18629=DIRECTION('ref_axis',(1.,0.,0.));
#18630=DIRECTION('center_axis',(0.,1.,0.));
#18631=DIRECTION('ref_axis',(1.,0.,0.));
#18632=DIRECTION('center_axis',(0.,-1.,0.));
#18633=DIRECTION('ref_axis',(0.,0.,-1.));
#18634=DIRECTION('center_axis',(0.,0.,1.));
#18635=DIRECTION('ref_axis',(1.,0.,0.));
#18636=DIRECTION('center_axis',(0.,-1.,0.));
#18637=DIRECTION('ref_axis',(0.,0.,-1.));
#18638=DIRECTION('center_axis',(0.,-1.,0.));
#18639=DIRECTION('ref_axis',(-1.,0.,0.));
#18640=DIRECTION('center_axis',(0.,1.,0.));
#18641=DIRECTION('ref_axis',(1.,0.,0.));
#18642=DIRECTION('axis',(0.,0.,1.));
#18643=DIRECTION('refdir',(1.,0.,0.));
#18644=DIRECTION('center_axis',(0.,1.,0.));
#18645=DIRECTION('ref_axis',(0.,0.,1.));
#18646=DIRECTION('center_axis',(0.,-1.,0.));
#18647=DIRECTION('ref_axis',(1.,0.,0.));
#18648=DIRECTION('center_axis',(0.,-1.,0.));
#18649=DIRECTION('ref_axis',(1.,0.,0.));
#18650=DIRECTION('center_axis',(0.,-1.,0.));
#18651=DIRECTION('ref_axis',(1.,0.,0.));
#18652=DIRECTION('center_axis',(0.,-1.,0.));
#18653=DIRECTION('ref_axis',(1.,0.,0.));
#18654=DIRECTION('',(0.,1.,0.));
#18655=DIRECTION('center_axis',(0.,-1.,0.));
#18656=DIRECTION('ref_axis',(0.,0.,-1.));
#18657=DIRECTION('center_axis',(0.,-1.,0.));
#18658=DIRECTION('ref_axis',(1.,0.,0.));
#18659=DIRECTION('center_axis',(0.,-1.,0.));
#18660=DIRECTION('ref_axis',(1.,0.,0.));
#18661=DIRECTION('',(0.,1.,0.));
#18662=DIRECTION('center_axis',(0.,1.,0.));
#18663=DIRECTION('ref_axis',(0.,0.,1.));
#18664=DIRECTION('center_axis',(0.,-1.,0.));
#18665=DIRECTION('ref_axis',(1.,0.,0.));
#18666=DIRECTION('center_axis',(0.,-1.,0.));
#18667=DIRECTION('ref_axis',(1.,0.,0.));
#18668=DIRECTION('center_axis',(0.,-1.,0.));
#18669=DIRECTION('ref_axis',(1.,0.,0.));
#18670=DIRECTION('center_axis',(0.,-1.,0.));
#18671=DIRECTION('ref_axis',(1.,0.,0.));
#18672=DIRECTION('',(0.,1.,0.));
#18673=DIRECTION('center_axis',(0.,-1.,0.));
#18674=DIRECTION('ref_axis',(0.,0.,-1.));
#18675=DIRECTION('center_axis',(0.,-1.,0.));
#18676=DIRECTION('ref_axis',(1.,0.,0.));
#18677=DIRECTION('center_axis',(0.,-1.,0.));
#18678=DIRECTION('ref_axis',(1.,0.,0.));
#18679=DIRECTION('',(0.,1.,0.));
#18680=DIRECTION('',(0.,0.,1.));
#18681=DIRECTION('',(1.,0.,0.));
#18682=DIRECTION('',(0.,0.,1.));
#18683=DIRECTION('',(1.,0.,0.));
#18684=DIRECTION('',(0.,0.,1.));
#18685=DIRECTION('',(1.,0.,0.));
#18686=DIRECTION('',(0.,0.,1.));
#18687=DIRECTION('',(1.,0.,0.));
#18688=DIRECTION('',(0.,0.,1.));
#18689=DIRECTION('',(1.,0.,0.));
#18690=DIRECTION('axis',(0.,0.,1.));
#18691=DIRECTION('refdir',(1.,0.,0.));
#18692=DIRECTION('center_axis',(0.,1.,0.));
#18693=DIRECTION('ref_axis',(0.,0.,1.));
#18694=DIRECTION('center_axis',(0.,-1.,0.));
#18695=DIRECTION('ref_axis',(1.,0.,0.));
#18696=DIRECTION('center_axis',(0.,-1.,0.));
#18697=DIRECTION('ref_axis',(1.,0.,0.));
#18698=DIRECTION('center_axis',(0.,-1.,0.));
#18699=DIRECTION('ref_axis',(1.,0.,0.));
#18700=DIRECTION('',(0.707106781186548,0.707106781186547,8.65956056235493E-17));
#18701=DIRECTION('center_axis',(0.,-1.,0.));
#18702=DIRECTION('ref_axis',(1.,0.,0.));
#18703=DIRECTION('center_axis',(0.,-1.,0.));
#18704=DIRECTION('ref_axis',(1.,0.,0.));
#18705=DIRECTION('',(0.,1.,0.));
#18706=DIRECTION('center_axis',(0.,1.,0.));
#18707=DIRECTION('ref_axis',(1.,0.,0.));
#18708=DIRECTION('center_axis',(0.,-1.,0.));
#18709=DIRECTION('ref_axis',(1.,0.,0.));
#18710=DIRECTION('',(-0.707106781186547,0.707106781186548,-8.65956056235493E-17));
#18711=DIRECTION('center_axis',(0.,-1.,0.));
#18712=DIRECTION('ref_axis',(0.,0.,-1.));
#18713=DIRECTION('center_axis',(0.,-1.,0.));
#18714=DIRECTION('ref_axis',(1.,0.,0.));
#18715=DIRECTION('center_axis',(0.,1.,0.));
#18716=DIRECTION('ref_axis',(1.,0.,0.));
#18717=DIRECTION('center_axis',(0.,1.,0.));
#18718=DIRECTION('ref_axis',(1.,0.,0.));
#18719=DIRECTION('',(-0.447213595499958,0.894427190999916,-5.47678698264203E-17));
#18720=DIRECTION('center_axis',(0.,-1.,0.));
#18721=DIRECTION('ref_axis',(1.,0.,0.));
#18722=DIRECTION('center_axis',(0.,1.,0.));
#18723=DIRECTION('ref_axis',(1.,0.,0.));
#18724=DIRECTION('',(0.,1.,0.));
#18725=DIRECTION('center_axis',(0.,1.,0.));
#18726=DIRECTION('ref_axis',(1.,0.,0.));
#18727=DIRECTION('center_axis',(0.,-1.,0.));
#18728=DIRECTION('ref_axis',(1.,0.,0.));
#18729=DIRECTION('',(-0.707106781186547,0.707106781186548,-8.65956056235493E-17));
#18730=DIRECTION('center_axis',(0.,-1.,0.));
#18731=DIRECTION('ref_axis',(0.,0.,-1.));
#18732=DIRECTION('center_axis',(0.866025403784439,0.,-0.5));
#18733=DIRECTION('ref_axis',(0.5,0.,0.866025403784439));
#18734=DIRECTION('',(-0.5,0.,-0.866025403784439));
#18735=DIRECTION('',(0.,-1.,0.));
#18736=DIRECTION('',(0.5,0.,0.866025403784439));
#18737=DIRECTION('',(0.,-1.,0.));
#18738=DIRECTION('center_axis',(1.20185167898973E-16,0.,-1.));
#18739=DIRECTION('ref_axis',(1.,0.,1.20185167898973E-16));
#18740=DIRECTION('',(-1.,0.,-1.20185167898973E-16));
#18741=DIRECTION('',(0.,-1.,0.));
#18742=DIRECTION('',(1.,0.,1.20185167898973E-16));
#18743=DIRECTION('center_axis',(-0.866025403784439,0.,-0.5));
#18744=DIRECTION('ref_axis',(0.5,0.,-0.866025403784439));
#18745=DIRECTION('',(-0.5,0.,0.866025403784439));
#18746=DIRECTION('',(0.,-1.,0.));
#18747=DIRECTION('',(0.5,0.,-0.866025403784439));
#18748=DIRECTION('center_axis',(-0.866025403784439,0.,0.5));
#18749=DIRECTION('ref_axis',(-0.5,0.,-0.866025403784439));
#18750=DIRECTION('',(0.5,0.,0.866025403784439));
#18751=DIRECTION('',(0.,-1.,0.));
#18752=DIRECTION('',(-0.5,0.,-0.866025403784439));
#18753=DIRECTION('center_axis',(-2.40370335797945E-16,0.,1.));
#18754=DIRECTION('ref_axis',(-1.,0.,-2.40370335797945E-16));
#18755=DIRECTION('',(1.,0.,2.40370335797945E-16));
#18756=DIRECTION('',(0.,-1.,0.));
#18757=DIRECTION('',(-1.,0.,-2.40370335797945E-16));
#18758=DIRECTION('center_axis',(0.866025403784439,0.,0.5));
#18759=DIRECTION('ref_axis',(-0.5,0.,0.866025403784439));
#18760=DIRECTION('',(0.5,0.,-0.866025403784439));
#18761=DIRECTION('',(-0.5,0.,0.866025403784439));
#18762=DIRECTION('center_axis',(0.,1.,0.));
#18763=DIRECTION('ref_axis',(1.,0.,0.));
#18764=DIRECTION('center_axis',(0.,-1.,0.));
#18765=DIRECTION('ref_axis',(0.,0.,-1.));
#18766=DIRECTION('axis',(0.,0.,1.));
#18767=DIRECTION('refdir',(1.,0.,0.));
#18768=DIRECTION('axis',(0.,0.,1.));
#18769=DIRECTION('refdir',(1.,0.,0.));
#18770=DIRECTION('center_axis',(0.,1.,0.));
#18771=DIRECTION('ref_axis',(1.,0.,0.));
#18772=DIRECTION('center_axis',(0.,1.,0.));
#18773=DIRECTION('ref_axis',(1.,0.,0.));
#18774=DIRECTION('',(0.,1.,0.));
#18775=DIRECTION('center_axis',(0.,-1.,0.));
#18776=DIRECTION('ref_axis',(1.,0.,0.));
#18777=DIRECTION('center_axis',(0.,1.,0.));
#18778=DIRECTION('ref_axis',(1.,0.,0.));
#18779=DIRECTION('center_axis',(0.,1.,0.));
#18780=DIRECTION('ref_axis',(1.,0.,0.));
#18781=DIRECTION('',(0.,1.,0.));
#18782=DIRECTION('center_axis',(0.,-1.,0.));
#18783=DIRECTION('ref_axis',(1.,0.,0.));
#18784=DIRECTION('center_axis',(6.12323399573677E-17,0.,1.));
#18785=DIRECTION('ref_axis',(1.,0.,0.));
#18786=DIRECTION('center_axis',(-1.22464679914735E-16,1.,0.));
#18787=DIRECTION('ref_axis',(-1.,-1.22464679914735E-16,0.));
#18788=DIRECTION('center_axis',(0.,1.,0.));
#18789=DIRECTION('ref_axis',(0.,0.,1.));
#18790=DIRECTION('',(1.,0.,0.));
#18791=DIRECTION('',(0.850265146687862,0.,0.526354614616295));
#18792=DIRECTION('center_axis',(0.,1.,0.));
#18793=DIRECTION('ref_axis',(1.,0.,0.));
#18794=DIRECTION('center_axis',(0.,1.,0.));
#18795=DIRECTION('ref_axis',(0.,0.,1.));
#18796=DIRECTION('',(1.,0.,0.));
#18797=DIRECTION('center_axis',(0.,1.,0.));
#18798=DIRECTION('ref_axis',(1.,0.,0.));
#18799=DIRECTION('',(0.850265146687862,0.,-0.526354614616295));
#18800=DIRECTION('center_axis',(0.,-1.,0.));
#18801=DIRECTION('ref_axis',(0.,0.,-1.));
#18802=DIRECTION('',(-1.,0.,0.));
#18803=DIRECTION('center_axis',(0.,-1.,0.));
#18804=DIRECTION('ref_axis',(1.,0.,0.));
#18805=DIRECTION('',(-0.850265146687862,0.,-0.526354614616295));
#18806=DIRECTION('center_axis',(-0.526354614616295,0.,0.850265146687862));
#18807=DIRECTION('ref_axis',(0.850265146687862,0.,0.526354614616295));
#18808=DIRECTION('',(0.,1.,0.));
#18809=DIRECTION('',(0.,-1.,0.));
#18810=DIRECTION('center_axis',(0.,-1.,0.));
#18811=DIRECTION('ref_axis',(0.,0.,-1.));
#18812=DIRECTION('',(-1.,0.,0.));
#18813=DIRECTION('',(-0.850265146687862,0.,0.526354614616295));
#18814=DIRECTION('center_axis',(0.,-1.,0.));
#18815=DIRECTION('ref_axis',(1.,0.,0.));
#18816=DIRECTION('center_axis',(0.526354614616295,0.,0.850265146687862));
#18817=DIRECTION('ref_axis',(0.850265146687862,0.,-0.526354614616295));
#18818=DIRECTION('',(0.,-1.,0.));
#18819=DIRECTION('',(0.,1.,0.));
#18820=DIRECTION('center_axis',(0.,0.,1.));
#18821=DIRECTION('ref_axis',(1.,0.,0.));
#18822=DIRECTION('',(0.,-1.,0.));
#18823=DIRECTION('',(1.,0.,0.));
#18824=DIRECTION('',(0.,1.,0.));
#18825=DIRECTION('',(-1.,0.,0.));
#18826=DIRECTION('center_axis',(0.,0.,-1.));
#18827=DIRECTION('ref_axis',(1.,0.,0.));
#18828=DIRECTION('center_axis',(0.,0.,-1.));
#18829=DIRECTION('ref_axis',(1.,0.,0.));
#18830=DIRECTION('',(0.,-1.,0.));
#18831=DIRECTION('',(-1.,0.,0.));
#18832=DIRECTION('',(0.,1.,0.));
#18833=DIRECTION('',(0.,1.,0.));
#18834=DIRECTION('',(1.,0.,0.));
#18835=DIRECTION('',(0.,-1.,0.));
#18836=DIRECTION('center_axis',(0.,1.,0.));
#18837=DIRECTION('ref_axis',(6.12323399573677E-17,0.,1.));
#18838=DIRECTION('center_axis',(0.,1.,0.));
#18839=DIRECTION('ref_axis',(1.,0.,0.));
#18840=DIRECTION('center_axis',(0.,-1.,0.));
#18841=DIRECTION('ref_axis',(1.,0.,0.));
#18842=DIRECTION('center_axis',(0.,1.,0.));
#18843=DIRECTION('ref_axis',(1.,0.,0.));
#18844=DIRECTION('center_axis',(0.,1.,0.));
#18845=DIRECTION('ref_axis',(1.,0.,0.));
#18846=DIRECTION('center_axis',(0.,1.,0.));
#18847=DIRECTION('ref_axis',(-1.,0.,0.));
#18848=DIRECTION('',(-1.,0.,0.));
#18849=DIRECTION('',(0.,0.,1.));
#18850=DIRECTION('',(-1.,0.,0.));
#18851=DIRECTION('',(0.,0.,1.));
#18852=DIRECTION('center_axis',(1.,0.,0.));
#18853=DIRECTION('ref_axis',(0.,1.,0.));
#18854=DIRECTION('',(0.,1.,0.));
#18855=DIRECTION('',(0.,0.,1.));
#18856=DIRECTION('',(0.,1.,0.));
#18857=DIRECTION('center_axis',(0.,-1.,0.));
#18858=DIRECTION('ref_axis',(1.,0.,0.));
#18859=DIRECTION('',(1.,0.,0.));
#18860=DIRECTION('',(0.,0.,1.));
#18861=DIRECTION('',(1.,0.,0.));
#18862=DIRECTION('center_axis',(-1.,0.,0.));
#18863=DIRECTION('ref_axis',(0.,-1.,0.));
#18864=DIRECTION('',(0.,-1.,0.));
#18865=DIRECTION('',(0.,-1.,0.));
#18866=DIRECTION('center_axis',(0.,0.,1.));
#18867=DIRECTION('ref_axis',(1.,0.,0.));
#18868=DIRECTION('center_axis',(0.,0.,1.));
#18869=DIRECTION('ref_axis',(1.,0.,0.));
#18870=DIRECTION('center_axis',(0.,0.,1.));
#18871=DIRECTION('ref_axis',(1.,0.,0.));
#18872=DIRECTION('',(0.,0.,1.));
#18873=DIRECTION('center_axis',(0.,0.,1.));
#18874=DIRECTION('ref_axis',(1.,0.,0.));
#18875=DIRECTION('center_axis',(0.,0.,1.));
#18876=DIRECTION('ref_axis',(1.,0.,0.));
#18877=DIRECTION('',(0.,0.,1.));
#18878=DIRECTION('center_axis',(0.,1.,0.));
#18879=DIRECTION('ref_axis',(-1.,0.,0.));
#18880=DIRECTION('',(-1.,0.,0.));
#18881=DIRECTION('',(0.,0.,1.));
#18882=DIRECTION('',(0.,0.,1.));
#18883=DIRECTION('center_axis',(1.,0.,0.));
#18884=DIRECTION('ref_axis',(0.,1.,0.));
#18885=DIRECTION('',(0.,1.,0.));
#18886=DIRECTION('',(0.,0.,1.));
#18887=DIRECTION('center_axis',(0.,-1.,0.));
#18888=DIRECTION('ref_axis',(1.,0.,0.));
#18889=DIRECTION('',(1.,0.,0.));
#18890=DIRECTION('',(0.,0.,1.));
#18891=DIRECTION('center_axis',(-1.,0.,0.));
#18892=DIRECTION('ref_axis',(0.,-1.,0.));
#18893=DIRECTION('',(0.,-1.,0.));
#18894=DIRECTION('center_axis',(0.,0.,1.));
#18895=DIRECTION('ref_axis',(1.,0.,0.));
#18896=DIRECTION('axis',(0.,0.,1.));
#18897=DIRECTION('refdir',(1.,0.,0.));
#18898=DIRECTION('center_axis',(0.,-1.,0.));
#18899=DIRECTION('ref_axis',(1.,0.,0.));
#18900=DIRECTION('center_axis',(0.,-1.,0.));
#18901=DIRECTION('ref_axis',(1.,0.,0.));
#18902=DIRECTION('',(0.,1.,0.));
#18903=DIRECTION('center_axis',(0.,-1.,0.));
#18904=DIRECTION('ref_axis',(1.,0.,0.));
#18905=DIRECTION('center_axis',(0.,1.,0.));
#18906=DIRECTION('ref_axis',(0.,0.,1.));
#18907=DIRECTION('center_axis',(0.,-1.,0.));
#18908=DIRECTION('ref_axis',(1.,0.,0.));
#18909=DIRECTION('center_axis',(6.12323399573677E-17,0.,1.));
#18910=DIRECTION('ref_axis',(1.,0.,0.));
#18911=DIRECTION('center_axis',(1.22464679914735E-16,-1.,0.));
#18912=DIRECTION('ref_axis',(-1.,-1.22464679914735E-16,0.));
#18913=DIRECTION('center_axis',(0.,-1.,0.));
#18914=DIRECTION('ref_axis',(1.,0.,0.));
#18915=DIRECTION('center_axis',(0.,-1.,0.));
#18916=DIRECTION('ref_axis',(0.,0.,-1.));
#18917=DIRECTION('center_axis',(-0.866025403784438,0.,-0.5));
#18918=DIRECTION('ref_axis',(-0.5,0.,0.866025403784438));
#18919=DIRECTION('',(-0.866025403784438,0.,-0.5));
#18920=DIRECTION('center_axis',(-0.866025403784438,0.,-0.5));
#18921=DIRECTION('ref_axis',(-0.5,0.,0.866025403784438));
#18922=DIRECTION('',(-0.866025403784438,0.,-0.5));
#18923=DIRECTION('center_axis',(0.,-1.,0.));
#18924=DIRECTION('ref_axis',(1.,0.,0.));
#18925=DIRECTION('center_axis',(0.,-1.,0.));
#18926=DIRECTION('ref_axis',(1.,0.,0.));
#18927=DIRECTION('',(0.,1.,0.));
#18928=DIRECTION('center_axis',(0.,-1.,0.));
#18929=DIRECTION('ref_axis',(1.,0.,0.));
#18930=DIRECTION('center_axis',(0.866025403784439,0.,-0.5));
#18931=DIRECTION('ref_axis',(-0.5,0.,-0.866025403784439));
#18932=DIRECTION('',(0.866025403784439,0.,-0.5));
#18933=DIRECTION('center_axis',(0.866025403784439,0.,-0.5));
#18934=DIRECTION('ref_axis',(-0.5,0.,-0.866025403784439));
#18935=DIRECTION('',(0.866025403784439,0.,-0.5));
#18936=DIRECTION('center_axis',(0.,0.,1.));
#18937=DIRECTION('ref_axis',(1.,0.,0.));
#18938=DIRECTION('',(0.,0.,1.));
#18939=DIRECTION('center_axis',(0.,0.,1.));
#18940=DIRECTION('ref_axis',(1.,0.,0.));
#18941=DIRECTION('',(0.,0.,1.));
#18942=DIRECTION('center_axis',(0.,1.,0.));
#18943=DIRECTION('ref_axis',(0.,0.,1.));
#18944=DIRECTION('center_axis',(0.,-1.,0.));
#18945=DIRECTION('ref_axis',(1.,0.,0.));
#18946=DIRECTION('center_axis',(0.,1.,0.));
#18947=DIRECTION('ref_axis',(0.,0.,1.));
#18948=DIRECTION('center_axis',(0.,-1.,0.));
#18949=DIRECTION('ref_axis',(1.,0.,0.));
#18950=DIRECTION('center_axis',(0.,-1.,0.));
#18951=DIRECTION('ref_axis',(1.,0.,0.));
#18952=DIRECTION('center_axis',(0.,-1.,0.));
#18953=DIRECTION('ref_axis',(1.,0.,0.));
#18954=DIRECTION('',(0.,1.,0.));
#18955=DIRECTION('center_axis',(0.,-1.,0.));
#18956=DIRECTION('ref_axis',(0.,0.,-1.));
#18957=DIRECTION('center_axis',(0.,-1.,0.));
#18958=DIRECTION('ref_axis',(1.,0.,0.));
#18959=DIRECTION('center_axis',(0.,-1.,0.));
#18960=DIRECTION('ref_axis',(1.,0.,0.));
#18961=DIRECTION('',(0.,1.,0.));
#18962=DIRECTION('',(0.,0.,1.));
#18963=DIRECTION('',(1.,0.,0.));
#18964=DIRECTION('',(0.,0.,1.));
#18965=DIRECTION('',(1.,0.,0.));
#18966=DIRECTION('axis',(0.,0.,1.));
#18967=DIRECTION('refdir',(1.,0.,0.));
#18968=DIRECTION('center_axis',(0.,1.,0.));
#18969=DIRECTION('ref_axis',(1.,0.,0.));
#18970=DIRECTION('center_axis',(0.,-1.,0.));
#18971=DIRECTION('ref_axis',(1.,0.,0.));
#18972=DIRECTION('',(0.,-1.,0.));
#18973=DIRECTION('center_axis',(0.,-1.,0.));
#18974=DIRECTION('ref_axis',(1.,0.,0.));
#18975=DIRECTION('center_axis',(0.,1.,0.));
#18976=DIRECTION('ref_axis',(1.,0.,0.));
#18977=DIRECTION('center_axis',(0.,1.,0.));
#18978=DIRECTION('ref_axis',(1.,0.,0.));
#18979=DIRECTION('',(0.,-1.,0.));
#18980=DIRECTION('center_axis',(0.,1.,0.));
#18981=DIRECTION('ref_axis',(1.,0.,0.));
#18982=DIRECTION('center_axis',(0.,1.,0.));
#18983=DIRECTION('ref_axis',(1.,0.,0.));
#18984=DIRECTION('center_axis',(0.,1.,0.));
#18985=DIRECTION('ref_axis',(1.,0.,0.));
#18986=DIRECTION('axis',(0.,0.,1.));
#18987=DIRECTION('refdir',(1.,0.,0.));
#18988=DIRECTION('center_axis',(0.866025403784439,0.,-0.5));
#18989=DIRECTION('ref_axis',(0.5,0.,0.866025403784439));
#18990=DIRECTION('',(-0.5,0.,-0.866025403784439));
#18991=DIRECTION('',(0.,-1.,0.));
#18992=DIRECTION('',(0.5,0.,0.866025403784439));
#18993=DIRECTION('',(0.,-1.,0.));
#18994=DIRECTION('center_axis',(1.60246890531964E-16,0.,-1.));
#18995=DIRECTION('ref_axis',(1.,0.,1.60246890531964E-16));
#18996=DIRECTION('',(-1.,0.,-1.60246890531964E-16));
#18997=DIRECTION('',(0.,-1.,0.));
#18998=DIRECTION('',(1.,0.,1.60246890531964E-16));
#18999=DIRECTION('center_axis',(-0.866025403784439,0.,-0.5));
#19000=DIRECTION('ref_axis',(0.5,0.,-0.866025403784439));
#19001=DIRECTION('',(-0.5,0.,0.866025403784439));
#19002=DIRECTION('',(0.,-1.,0.));
#19003=DIRECTION('',(0.5,0.,-0.866025403784439));
#19004=DIRECTION('center_axis',(-0.866025403784439,0.,0.5));
#19005=DIRECTION('ref_axis',(-0.5,0.,-0.866025403784439));
#19006=DIRECTION('',(0.5,0.,0.866025403784439));
#19007=DIRECTION('',(0.,-1.,0.));
#19008=DIRECTION('',(-0.5,0.,-0.866025403784439));
#19009=DIRECTION('center_axis',(-1.60246890531964E-16,0.,1.));
#19010=DIRECTION('ref_axis',(-1.,0.,-1.60246890531964E-16));
#19011=DIRECTION('',(1.,0.,1.60246890531964E-16));
#19012=DIRECTION('',(0.,-1.,0.));
#19013=DIRECTION('',(-1.,0.,-1.60246890531964E-16));
#19014=DIRECTION('center_axis',(0.866025403784439,0.,0.5));
#19015=DIRECTION('ref_axis',(-0.5,0.,0.866025403784439));
#19016=DIRECTION('',(0.5,0.,-0.866025403784439));
#19017=DIRECTION('',(-0.5,0.,0.866025403784439));
#19018=DIRECTION('center_axis',(0.,1.,0.));
#19019=DIRECTION('ref_axis',(1.,0.,0.));
#19020=DIRECTION('center_axis',(0.,-1.,0.));
#19021=DIRECTION('ref_axis',(0.,0.,-1.));
#19022=DIRECTION('center_axis',(0.,1.,0.));
#19023=DIRECTION('ref_axis',(1.,0.,0.));
#19024=DIRECTION('center_axis',(0.,1.,0.));
#19025=DIRECTION('ref_axis',(1.,0.,0.));
#19026=DIRECTION('center_axis',(0.,1.,0.));
#19027=DIRECTION('ref_axis',(0.,0.,1.));
#19028=DIRECTION('center_axis',(0.,-1.,0.));
#19029=DIRECTION('ref_axis',(1.,0.,0.));
#19030=DIRECTION('center_axis',(0.,-1.,0.));
#19031=DIRECTION('ref_axis',(1.,0.,0.));
#19032=DIRECTION('center_axis',(0.,-1.,0.));
#19033=DIRECTION('ref_axis',(1.,0.,0.));
#19034=DIRECTION('',(0.707106781186548,0.707106781186547,8.65956056235493E-17));
#19035=DIRECTION('center_axis',(0.,-1.,0.));
#19036=DIRECTION('ref_axis',(1.,0.,0.));
#19037=DIRECTION('center_axis',(0.,-1.,0.));
#19038=DIRECTION('ref_axis',(1.,0.,0.));
#19039=DIRECTION('',(0.,1.,0.));
#19040=DIRECTION('center_axis',(0.,1.,0.));
#19041=DIRECTION('ref_axis',(1.,0.,0.));
#19042=DIRECTION('center_axis',(0.,-1.,0.));
#19043=DIRECTION('ref_axis',(1.,0.,0.));
#19044=DIRECTION('',(-0.707106781186548,0.707106781186547,-8.65956056235494E-17));
#19045=DIRECTION('center_axis',(0.,-1.,0.));
#19046=DIRECTION('ref_axis',(0.,0.,-1.));
#19047=DIRECTION('center_axis',(0.,-1.,0.));
#19048=DIRECTION('ref_axis',(1.,0.,0.));
#19049=DIRECTION('center_axis',(0.,1.,0.));
#19050=DIRECTION('ref_axis',(1.,0.,0.));
#19051=DIRECTION('center_axis',(0.,1.,0.));
#19052=DIRECTION('ref_axis',(1.,0.,0.));
#19053=DIRECTION('',(-0.447213595499958,0.894427190999916,-5.47678698264203E-17));
#19054=DIRECTION('center_axis',(0.,-1.,0.));
#19055=DIRECTION('ref_axis',(1.,0.,0.));
#19056=DIRECTION('',(0.,1.,0.));
#19057=DIRECTION('axis',(0.,0.,1.));
#19058=DIRECTION('refdir',(1.,0.,0.));
#19059=DIRECTION('center_axis',(0.866025403784439,0.,-0.5));
#19060=DIRECTION('ref_axis',(0.5,0.,0.866025403784439));
#19061=DIRECTION('',(-0.5,0.,-0.866025403784439));
#19062=DIRECTION('',(0.,-1.,0.));
#19063=DIRECTION('',(0.5,0.,0.866025403784439));
#19064=DIRECTION('',(0.,-1.,0.));
#19065=DIRECTION('center_axis',(1.60246890531964E-16,0.,-1.));
#19066=DIRECTION('ref_axis',(1.,0.,1.60246890531964E-16));
#19067=DIRECTION('',(-1.,0.,-1.60246890531964E-16));
#19068=DIRECTION('',(0.,-1.,0.));
#19069=DIRECTION('',(1.,0.,1.60246890531964E-16));
#19070=DIRECTION('center_axis',(-0.866025403784439,0.,-0.5));
#19071=DIRECTION('ref_axis',(0.5,0.,-0.866025403784439));
#19072=DIRECTION('',(-0.5,0.,0.866025403784439));
#19073=DIRECTION('',(0.,-1.,0.));
#19074=DIRECTION('',(0.5,0.,-0.866025403784439));
#19075=DIRECTION('center_axis',(-0.866025403784439,0.,0.5));
#19076=DIRECTION('ref_axis',(-0.5,0.,-0.866025403784439));
#19077=DIRECTION('',(0.5,0.,0.866025403784439));
#19078=DIRECTION('',(0.,-1.,0.));
#19079=DIRECTION('',(-0.5,0.,-0.866025403784439));
#19080=DIRECTION('center_axis',(-1.60246890531964E-16,0.,1.));
#19081=DIRECTION('ref_axis',(-1.,0.,-1.60246890531964E-16));
#19082=DIRECTION('',(1.,0.,1.60246890531964E-16));
#19083=DIRECTION('',(0.,-1.,0.));
#19084=DIRECTION('',(-1.,0.,-1.60246890531964E-16));
#19085=DIRECTION('center_axis',(0.866025403784439,0.,0.5));
#19086=DIRECTION('ref_axis',(-0.5,0.,0.866025403784439));
#19087=DIRECTION('',(0.5,0.,-0.866025403784439));
#19088=DIRECTION('',(-0.5,0.,0.866025403784439));
#19089=DIRECTION('center_axis',(0.,1.,0.));
#19090=DIRECTION('ref_axis',(1.,0.,0.));
#19091=DIRECTION('center_axis',(0.,-1.,0.));
#19092=DIRECTION('ref_axis',(0.,0.,-1.));
#19093=DIRECTION('center_axis',(0.,1.,0.));
#19094=DIRECTION('ref_axis',(1.,0.,0.));
#19095=DIRECTION('center_axis',(0.,1.,0.));
#19096=DIRECTION('ref_axis',(1.,0.,0.));
#19097=DIRECTION('center_axis',(0.,1.,0.));
#19098=DIRECTION('ref_axis',(0.,0.,1.));
#19099=DIRECTION('center_axis',(0.,-1.,0.));
#19100=DIRECTION('ref_axis',(1.,0.,0.));
#19101=DIRECTION('center_axis',(0.,-1.,0.));
#19102=DIRECTION('ref_axis',(1.,0.,0.));
#19103=DIRECTION('center_axis',(0.,-1.,0.));
#19104=DIRECTION('ref_axis',(1.,0.,0.));
#19105=DIRECTION('',(0.707106781186547,0.707106781186548,8.65956056235493E-17));
#19106=DIRECTION('center_axis',(0.,-1.,0.));
#19107=DIRECTION('ref_axis',(1.,0.,0.));
#19108=DIRECTION('center_axis',(0.,-1.,0.));
#19109=DIRECTION('ref_axis',(1.,0.,0.));
#19110=DIRECTION('',(0.,1.,0.));
#19111=DIRECTION('center_axis',(0.,1.,0.));
#19112=DIRECTION('ref_axis',(1.,0.,0.));
#19113=DIRECTION('center_axis',(0.,-1.,0.));
#19114=DIRECTION('ref_axis',(1.,0.,0.));
#19115=DIRECTION('',(-0.707106781186547,0.707106781186548,-8.65956056235493E-17));
#19116=DIRECTION('center_axis',(0.,-1.,0.));
#19117=DIRECTION('ref_axis',(0.,0.,-1.));
#19118=DIRECTION('center_axis',(0.,-1.,0.));
#19119=DIRECTION('ref_axis',(1.,0.,0.));
#19120=DIRECTION('center_axis',(0.,1.,0.));
#19121=DIRECTION('ref_axis',(1.,0.,0.));
#19122=DIRECTION('center_axis',(0.,1.,0.));
#19123=DIRECTION('ref_axis',(1.,0.,0.));
#19124=DIRECTION('',(-0.447213595499958,0.894427190999916,-5.47678698264203E-17));
#19125=DIRECTION('center_axis',(0.,-1.,0.));
#19126=DIRECTION('ref_axis',(1.,0.,0.));
#19127=DIRECTION('',(0.,1.,0.));
#19128=DIRECTION('axis',(0.,0.,1.));
#19129=DIRECTION('refdir',(1.,0.,0.));
#19130=DIRECTION('axis',(0.,0.,1.));
#19131=DIRECTION('refdir',(1.,0.,0.));
#19132=DIRECTION('center_axis',(0.,1.,0.));
#19133=DIRECTION('ref_axis',(1.,0.,0.));
#19134=DIRECTION('center_axis',(0.,1.,0.));
#19135=DIRECTION('ref_axis',(1.,0.,0.));
#19136=DIRECTION('',(0.,1.,0.));
#19137=DIRECTION('center_axis',(0.,1.,0.));
#19138=DIRECTION('ref_axis',(1.,0.,0.));
#19139=DIRECTION('center_axis',(0.,1.,0.));
#19140=DIRECTION('ref_axis',(1.,0.,0.));
#19141=DIRECTION('center_axis',(0.,1.,0.));
#19142=DIRECTION('ref_axis',(1.,0.,0.));
#19143=DIRECTION('center_axis',(0.,1.,0.));
#19144=DIRECTION('ref_axis',(1.,0.,0.));
#19145=DIRECTION('center_axis',(0.,1.,0.));
#19146=DIRECTION('ref_axis',(1.,0.,0.));
#19147=DIRECTION('center_axis',(0.,1.,0.));
#19148=DIRECTION('ref_axis',(1.,0.,0.));
#19149=DIRECTION('center_axis',(0.,1.,0.));
#19150=DIRECTION('ref_axis',(1.,0.,0.));
#19151=DIRECTION('center_axis',(0.,-1.,0.));
#19152=DIRECTION('ref_axis',(1.,0.,0.));
#19153=DIRECTION('center_axis',(0.,1.,0.));
#19154=DIRECTION('ref_axis',(1.,0.,0.));
#19155=DIRECTION('',(0.,-1.,0.));
#19156=DIRECTION('center_axis',(0.,1.,0.));
#19157=DIRECTION('ref_axis',(1.,0.,0.));
#19158=DIRECTION('',(0.,-1.,0.));
#19159=DIRECTION('center_axis',(0.,1.,0.));
#19160=DIRECTION('ref_axis',(1.,0.,0.));
#19161=DIRECTION('center_axis',(0.,1.,0.));
#19162=DIRECTION('ref_axis',(1.,0.,0.));
#19163=DIRECTION('center_axis',(0.,1.,0.));
#19164=DIRECTION('ref_axis',(1.,0.,0.));
#19165=DIRECTION('',(0.,-1.,0.));
#19166=DIRECTION('center_axis',(0.,1.,0.));
#19167=DIRECTION('ref_axis',(1.,0.,0.));
#19168=DIRECTION('center_axis',(0.,1.,0.));
#19169=DIRECTION('ref_axis',(1.,0.,0.));
#19170=DIRECTION('center_axis',(0.,1.,0.));
#19171=DIRECTION('ref_axis',(1.,0.,0.));
#19172=DIRECTION('center_axis',(0.,1.,0.));
#19173=DIRECTION('ref_axis',(1.,0.,0.));
#19174=DIRECTION('',(0.,-1.,0.));
#19175=DIRECTION('center_axis',(0.,1.,0.));
#19176=DIRECTION('ref_axis',(1.,0.,0.));
#19177=DIRECTION('center_axis',(0.,1.,0.));
#19178=DIRECTION('ref_axis',(1.,0.,0.));
#19179=DIRECTION('axis',(0.,0.,1.));
#19180=DIRECTION('refdir',(1.,0.,0.));
#19181=DIRECTION('center_axis',(0.,1.,0.));
#19182=DIRECTION('ref_axis',(1.,0.,0.));
#19183=DIRECTION('center_axis',(0.,1.,0.));
#19184=DIRECTION('ref_axis',(1.,0.,0.));
#19185=DIRECTION('',(0.,1.,0.));
#19186=DIRECTION('center_axis',(0.,-1.,0.));
#19187=DIRECTION('ref_axis',(1.,0.,0.));
#19188=DIRECTION('center_axis',(0.,1.,0.));
#19189=DIRECTION('ref_axis',(1.,0.,0.));
#19190=DIRECTION('center_axis',(0.,1.,0.));
#19191=DIRECTION('ref_axis',(1.,0.,0.));
#19192=DIRECTION('center_axis',(0.,1.,0.));
#19193=DIRECTION('ref_axis',(1.,0.,0.));
#19194=DIRECTION('',(0.,-1.,0.));
#19195=DIRECTION('center_axis',(0.,-1.,0.));
#19196=DIRECTION('ref_axis',(1.,0.,0.));
#19197=DIRECTION('center_axis',(0.,1.,0.));
#19198=DIRECTION('ref_axis',(1.,0.,0.));
#19199=DIRECTION('center_axis',(0.,1.,0.));
#19200=DIRECTION('ref_axis',(1.,0.,0.));
#19201=DIRECTION('',(0.,-1.,0.));
#19202=DIRECTION('center_axis',(0.,1.,0.));
#19203=DIRECTION('ref_axis',(1.,0.,0.));
#19204=DIRECTION('center_axis',(0.,1.,0.));
#19205=DIRECTION('ref_axis',(1.,0.,0.));
#19206=DIRECTION('center_axis',(0.,1.,0.));
#19207=DIRECTION('ref_axis',(1.,0.,0.));
#19208=DIRECTION('axis',(0.,0.,1.));
#19209=DIRECTION('refdir',(1.,0.,0.));
#19210=DIRECTION('center_axis',(0.,1.,0.));
#19211=DIRECTION('ref_axis',(1.,0.,0.));
#19212=DIRECTION('center_axis',(0.,-1.,0.));
#19213=DIRECTION('ref_axis',(1.,0.,0.));
#19214=DIRECTION('',(0.,-1.,0.));
#19215=DIRECTION('center_axis',(0.,-1.,0.));
#19216=DIRECTION('ref_axis',(1.,0.,0.));
#19217=DIRECTION('center_axis',(0.,1.,0.));
#19218=DIRECTION('ref_axis',(1.,0.,0.));
#19219=DIRECTION('center_axis',(0.,1.,0.));
#19220=DIRECTION('ref_axis',(1.,0.,0.));
#19221=DIRECTION('',(0.,-1.,0.));
#19222=DIRECTION('center_axis',(0.,1.,0.));
#19223=DIRECTION('ref_axis',(1.,0.,0.));
#19224=DIRECTION('center_axis',(0.,1.,0.));
#19225=DIRECTION('ref_axis',(1.,0.,0.));
#19226=DIRECTION('center_axis',(0.,1.,0.));
#19227=DIRECTION('ref_axis',(1.,0.,0.));
#19228=DIRECTION('axis',(0.,0.,1.));
#19229=DIRECTION('refdir',(1.,0.,0.));
#19230=DIRECTION('center_axis',(0.,0.,1.));
#19231=DIRECTION('ref_axis',(1.,0.,0.));
#19232=DIRECTION('center_axis',(0.,0.,1.));
#19233=DIRECTION('ref_axis',(1.,0.,0.));
#19234=DIRECTION('',(0.,0.,-1.));
#19235=DIRECTION('center_axis',(0.,0.,1.));
#19236=DIRECTION('ref_axis',(1.,0.,0.));
#19237=DIRECTION('center_axis',(0.,0.,1.));
#19238=DIRECTION('ref_axis',(1.,0.,0.));
#19239=DIRECTION('center_axis',(0.,0.,1.));
#19240=DIRECTION('ref_axis',(1.,0.,0.));
#19241=DIRECTION('axis',(0.,0.,1.));
#19242=DIRECTION('refdir',(1.,0.,0.));
#19243=DIRECTION('center_axis',(0.,0.,1.));
#19244=DIRECTION('ref_axis',(1.,0.,0.));
#19245=DIRECTION('center_axis',(0.,0.,1.));
#19246=DIRECTION('ref_axis',(1.,0.,0.));
#19247=DIRECTION('',(0.,0.,-1.));
#19248=DIRECTION('center_axis',(0.,0.,1.));
#19249=DIRECTION('ref_axis',(1.,0.,0.));
#19250=DIRECTION('center_axis',(0.,0.,1.));
#19251=DIRECTION('ref_axis',(1.,0.,0.));
#19252=DIRECTION('center_axis',(0.,0.,1.));
#19253=DIRECTION('ref_axis',(1.,0.,0.));
#19254=DIRECTION('axis',(0.,0.,1.));
#19255=DIRECTION('refdir',(1.,0.,0.));
#19256=DIRECTION('center_axis',(0.,1.,0.));
#19257=DIRECTION('ref_axis',(1.,0.,0.));
#19258=DIRECTION('center_axis',(0.,-1.,0.));
#19259=DIRECTION('ref_axis',(1.,0.,0.));
#19260=DIRECTION('',(0.,-1.,0.));
#19261=DIRECTION('center_axis',(0.,-1.,0.));
#19262=DIRECTION('ref_axis',(1.,0.,0.));
#19263=DIRECTION('center_axis',(0.,1.,0.));
#19264=DIRECTION('ref_axis',(1.,0.,0.));
#19265=DIRECTION('center_axis',(0.,1.,0.));
#19266=DIRECTION('ref_axis',(1.,0.,0.));
#19267=DIRECTION('',(0.,-1.,0.));
#19268=DIRECTION('center_axis',(0.,1.,0.));
#19269=DIRECTION('ref_axis',(1.,0.,0.));
#19270=DIRECTION('center_axis',(0.,1.,0.));
#19271=DIRECTION('ref_axis',(1.,0.,0.));
#19272=DIRECTION('center_axis',(0.,1.,0.));
#19273=DIRECTION('ref_axis',(1.,0.,0.));
#19274=DIRECTION('axis',(0.,0.,1.));
#19275=DIRECTION('refdir',(1.,0.,0.));
#19276=DIRECTION('center_axis',(0.,1.,0.));
#19277=DIRECTION('ref_axis',(1.,0.,0.));
#19278=DIRECTION('center_axis',(0.,1.,0.));
#19279=DIRECTION('ref_axis',(1.,0.,0.));
#19280=DIRECTION('',(0.,-1.,0.));
#19281=DIRECTION('center_axis',(0.,1.,0.));
#19282=DIRECTION('ref_axis',(1.,0.,0.));
#19283=DIRECTION('center_axis',(0.,1.,0.));
#19284=DIRECTION('ref_axis',(1.,0.,0.));
#19285=DIRECTION('center_axis',(0.,1.,0.));
#19286=DIRECTION('ref_axis',(1.,0.,0.));
#19287=DIRECTION('axis',(0.,0.,1.));
#19288=DIRECTION('refdir',(1.,0.,0.));
#19289=DIRECTION('center_axis',(0.,0.,1.));
#19290=DIRECTION('ref_axis',(1.,0.,0.));
#19291=DIRECTION('',(0.,1.,0.));
#19292=DIRECTION('center_axis',(0.,0.,1.));
#19293=DIRECTION('ref_axis',(1.,0.,0.));
#19294=DIRECTION('center_axis',(0.,0.,1.));
#19295=DIRECTION('ref_axis',(1.,0.,0.));
#19296=DIRECTION('center_axis',(0.,0.,1.));
#19297=DIRECTION('ref_axis',(1.,0.,0.));
#19298=DIRECTION('',(0.,0.,1.));
#19299=DIRECTION('center_axis',(0.,0.,1.));
#19300=DIRECTION('ref_axis',(1.,0.,0.));
#19301=DIRECTION('center_axis',(0.,0.,1.));
#19302=DIRECTION('ref_axis',(1.,0.,0.));
#19303=DIRECTION('',(0.,-1.,0.));
#19304=DIRECTION('center_axis',(0.,0.,1.));
#19305=DIRECTION('ref_axis',(1.,0.,0.));
#19306=DIRECTION('',(0.,1.,0.));
#19307=DIRECTION('center_axis',(0.,0.,1.));
#19308=DIRECTION('ref_axis',(1.,0.,0.));
#19309=DIRECTION('center_axis',(0.,0.,1.));
#19310=DIRECTION('ref_axis',(1.,0.,0.));
#19311=DIRECTION('center_axis',(0.,0.,1.));
#19312=DIRECTION('ref_axis',(1.,0.,0.));
#19313=DIRECTION('',(0.,0.,1.));
#19314=DIRECTION('center_axis',(0.,0.,1.));
#19315=DIRECTION('ref_axis',(1.,0.,0.));
#19316=DIRECTION('center_axis',(0.,0.,1.));
#19317=DIRECTION('ref_axis',(1.,0.,0.));
#19318=DIRECTION('',(0.,-1.,0.));
#19319=DIRECTION('center_axis',(0.,1.,0.));
#19320=DIRECTION('ref_axis',(1.,0.,0.));
#19321=DIRECTION('center_axis',(0.,-1.,0.));
#19322=DIRECTION('ref_axis',(1.,0.,0.));
#19323=DIRECTION('',(0.,-1.,0.));
#19324=DIRECTION('center_axis',(0.,-1.,0.));
#19325=DIRECTION('ref_axis',(1.,0.,0.));
#19326=DIRECTION('center_axis',(0.,1.,0.));
#19327=DIRECTION('ref_axis',(1.,0.,0.));
#19328=DIRECTION('center_axis',(0.,1.,0.));
#19329=DIRECTION('ref_axis',(1.,0.,0.));
#19330=DIRECTION('',(0.,-1.,0.));
#19331=DIRECTION('center_axis',(0.,1.,0.));
#19332=DIRECTION('ref_axis',(1.,0.,0.));
#19333=DIRECTION('center_axis',(0.,1.,0.));
#19334=DIRECTION('ref_axis',(1.,0.,0.));
#19335=DIRECTION('center_axis',(0.,1.,0.));
#19336=DIRECTION('ref_axis',(1.,0.,0.));
#19337=DIRECTION('axis',(0.,0.,1.));
#19338=DIRECTION('refdir',(1.,0.,0.));
#19339=DIRECTION('center_axis',(1.,0.,6.12323399573677E-17));
#19340=DIRECTION('ref_axis',(6.12323399573677E-17,0.,-1.));
#19341=DIRECTION('',(1.,0.,6.12323399573677E-17));
#19342=DIRECTION('center_axis',(1.,0.,6.12323399573677E-17));
#19343=DIRECTION('ref_axis',(6.12323399573677E-17,0.,-1.));
#19344=DIRECTION('',(1.,0.,6.12323399573677E-17));
#19345=DIRECTION('center_axis',(0.,-1.,0.));
#19346=DIRECTION('ref_axis',(1.,0.,0.));
#19347=DIRECTION('center_axis',(0.,-1.,0.));
#19348=DIRECTION('ref_axis',(1.,0.,0.));
#19349=DIRECTION('',(0.,1.,0.));
#19350=DIRECTION('',(0.,1.,0.));
#19351=DIRECTION('center_axis',(0.,1.,0.));
#19352=DIRECTION('ref_axis',(1.,0.,0.));
#19353=DIRECTION('center_axis',(0.,0.,1.));
#19354=DIRECTION('ref_axis',(1.,0.,0.));
#19355=DIRECTION('',(0.,0.,1.));
#19356=DIRECTION('center_axis',(0.,0.,1.));
#19357=DIRECTION('ref_axis',(1.,0.,0.));
#19358=DIRECTION('',(0.,0.,1.));
#19359=DIRECTION('center_axis',(0.,1.,0.));
#19360=DIRECTION('ref_axis',(1.,0.,0.));
#19361=DIRECTION('center_axis',(0.,1.,0.));
#19362=DIRECTION('ref_axis',(1.,0.,0.));
#19363=DIRECTION('',(0.,1.,0.));
#19364=DIRECTION('',(0.,1.,0.));
#19365=DIRECTION('center_axis',(0.,-1.,0.));
#19366=DIRECTION('ref_axis',(1.,0.,0.));
#19367=DIRECTION('center_axis',(0.,1.,0.));
#19368=DIRECTION('ref_axis',(1.,0.,0.));
#19369=DIRECTION('center_axis',(0.,1.,0.));
#19370=DIRECTION('ref_axis',(1.,0.,0.));
#19371=DIRECTION('center_axis',(0.,1.,0.));
#19372=DIRECTION('ref_axis',(1.,0.,0.));
#19373=DIRECTION('center_axis',(0.,1.,0.));
#19374=DIRECTION('ref_axis',(0.951056516295154,0.,0.309016994374948));
#19375=DIRECTION('center_axis',(0.,1.,0.));
#19376=DIRECTION('ref_axis',(1.,0.,0.));
#19377=DIRECTION('center_axis',(0.,1.,0.));
#19378=DIRECTION('ref_axis',(0.809016994374947,0.,0.587785252292473));
#19379=DIRECTION('center_axis',(0.,1.,0.));
#19380=DIRECTION('ref_axis',(1.,0.,0.));
#19381=DIRECTION('center_axis',(0.,1.,0.));
#19382=DIRECTION('ref_axis',(0.587785252292473,0.,0.809016994374948));
#19383=DIRECTION('center_axis',(0.,1.,0.));
#19384=DIRECTION('ref_axis',(1.,0.,0.));
#19385=DIRECTION('center_axis',(0.,1.,0.));
#19386=DIRECTION('ref_axis',(0.309016994374947,0.,0.951056516295154));
#19387=DIRECTION('center_axis',(0.,1.,0.));
#19388=DIRECTION('ref_axis',(1.,0.,0.));
#19389=DIRECTION('center_axis',(0.,1.,0.));
#19390=DIRECTION('ref_axis',(-1.83697019872103E-16,0.,1.));
#19391=DIRECTION('center_axis',(0.,1.,0.));
#19392=DIRECTION('ref_axis',(1.,0.,0.));
#19393=DIRECTION('center_axis',(0.,1.,0.));
#19394=DIRECTION('ref_axis',(-0.309016994374948,0.,0.951056516295154));
#19395=DIRECTION('center_axis',(0.,1.,0.));
#19396=DIRECTION('ref_axis',(1.,0.,0.));
#19397=DIRECTION('center_axis',(0.,1.,0.));
#19398=DIRECTION('ref_axis',(-0.587785252292473,0.,0.809016994374947));
#19399=DIRECTION('center_axis',(0.,1.,0.));
#19400=DIRECTION('ref_axis',(1.,0.,0.));
#19401=DIRECTION('center_axis',(0.,1.,0.));
#19402=DIRECTION('ref_axis',(-0.809016994374947,0.,0.587785252292473));
#19403=DIRECTION('center_axis',(0.,1.,0.));
#19404=DIRECTION('ref_axis',(1.,0.,0.));
#19405=DIRECTION('center_axis',(0.,1.,0.));
#19406=DIRECTION('ref_axis',(-0.951056516295154,0.,0.309016994374947));
#19407=DIRECTION('center_axis',(0.,1.,0.));
#19408=DIRECTION('ref_axis',(1.,0.,0.));
#19409=DIRECTION('center_axis',(0.,1.,0.));
#19410=DIRECTION('ref_axis',(-1.,0.,-1.22464679914735E-16));
#19411=DIRECTION('center_axis',(0.,1.,0.));
#19412=DIRECTION('ref_axis',(1.,0.,0.));
#19413=DIRECTION('center_axis',(0.,1.,0.));
#19414=DIRECTION('ref_axis',(-0.951056516295154,0.,-0.309016994374948));
#19415=DIRECTION('center_axis',(0.,1.,0.));
#19416=DIRECTION('ref_axis',(1.,0.,0.));
#19417=DIRECTION('center_axis',(0.,1.,0.));
#19418=DIRECTION('ref_axis',(-0.809016994374947,0.,-0.587785252292473));
#19419=DIRECTION('center_axis',(0.,1.,0.));
#19420=DIRECTION('ref_axis',(1.,0.,0.));
#19421=DIRECTION('center_axis',(0.,1.,0.));
#19422=DIRECTION('ref_axis',(-0.587785252292473,0.,-0.809016994374948));
#19423=DIRECTION('center_axis',(0.,1.,0.));
#19424=DIRECTION('ref_axis',(1.,0.,0.));
#19425=DIRECTION('center_axis',(0.,1.,0.));
#19426=DIRECTION('ref_axis',(-0.309016994374947,0.,-0.951056516295154));
#19427=DIRECTION('center_axis',(0.,1.,0.));
#19428=DIRECTION('ref_axis',(1.,0.,0.));
#19429=DIRECTION('center_axis',(0.,1.,0.));
#19430=DIRECTION('ref_axis',(6.12323399573677E-17,0.,-1.));
#19431=DIRECTION('center_axis',(0.,1.,0.));
#19432=DIRECTION('ref_axis',(1.,0.,0.));
#19433=DIRECTION('center_axis',(0.,1.,0.));
#19434=DIRECTION('ref_axis',(0.309016994374947,0.,-0.951056516295154));
#19435=DIRECTION('center_axis',(0.,1.,0.));
#19436=DIRECTION('ref_axis',(1.,0.,0.));
#19437=DIRECTION('center_axis',(0.,1.,0.));
#19438=DIRECTION('ref_axis',(0.587785252292473,0.,-0.809016994374947));
#19439=DIRECTION('center_axis',(0.,1.,0.));
#19440=DIRECTION('ref_axis',(1.,0.,0.));
#19441=DIRECTION('center_axis',(0.,1.,0.));
#19442=DIRECTION('ref_axis',(0.809016994374947,0.,-0.587785252292473));
#19443=DIRECTION('center_axis',(0.,1.,0.));
#19444=DIRECTION('ref_axis',(1.,0.,0.));
#19445=DIRECTION('center_axis',(0.,1.,0.));
#19446=DIRECTION('ref_axis',(0.951056516295154,0.,-0.309016994374947));
#19447=DIRECTION('center_axis',(0.,1.,0.));
#19448=DIRECTION('ref_axis',(1.,0.,0.));
#19449=DIRECTION('center_axis',(0.,1.,0.));
#19450=DIRECTION('ref_axis',(1.,0.,0.));
#19451=DIRECTION('center_axis',(0.,1.,0.));
#19452=DIRECTION('ref_axis',(1.,0.,0.));
#19453=DIRECTION('center_axis',(0.,-1.,0.));
#19454=DIRECTION('ref_axis',(1.,0.,0.));
#19455=DIRECTION('center_axis',(0.,-1.,0.));
#19456=DIRECTION('ref_axis',(1.,0.,0.));
#19457=DIRECTION('',(0.,1.,0.));
#19458=DIRECTION('center_axis',(0.,1.,0.));
#19459=DIRECTION('ref_axis',(1.,0.,0.));
#19460=DIRECTION('center_axis',(0.,1.,0.));
#19461=DIRECTION('ref_axis',(1.,0.,0.));
#19462=DIRECTION('center_axis',(0.,1.,0.));
#19463=DIRECTION('ref_axis',(1.,0.,0.));
#19464=DIRECTION('center_axis',(0.,-1.,0.));
#19465=DIRECTION('ref_axis',(0.951056516295154,0.,0.309016994374948));
#19466=DIRECTION('center_axis',(0.,1.,0.));
#19467=DIRECTION('ref_axis',(1.,0.,0.));
#19468=DIRECTION('center_axis',(0.,-1.,0.));
#19469=DIRECTION('ref_axis',(1.,0.,0.));
#19470=DIRECTION('center_axis',(0.,1.,0.));
#19471=DIRECTION('ref_axis',(1.,0.,0.));
#19472=DIRECTION('center_axis',(0.,-1.,0.));
#19473=DIRECTION('ref_axis',(0.951056516295154,0.,-0.309016994374947));
#19474=DIRECTION('center_axis',(0.,1.,0.));
#19475=DIRECTION('ref_axis',(1.,0.,0.));
#19476=DIRECTION('center_axis',(0.,-1.,0.));
#19477=DIRECTION('ref_axis',(0.809016994374947,0.,-0.587785252292473));
#19478=DIRECTION('center_axis',(0.,1.,0.));
#19479=DIRECTION('ref_axis',(1.,0.,0.));
#19480=DIRECTION('center_axis',(0.,-1.,0.));
#19481=DIRECTION('ref_axis',(0.587785252292473,0.,-0.809016994374947));
#19482=DIRECTION('center_axis',(0.,1.,0.));
#19483=DIRECTION('ref_axis',(1.,0.,0.));
#19484=DIRECTION('center_axis',(0.,-1.,0.));
#19485=DIRECTION('ref_axis',(0.309016994374947,0.,-0.951056516295154));
#19486=DIRECTION('center_axis',(0.,1.,0.));
#19487=DIRECTION('ref_axis',(1.,0.,0.));
#19488=DIRECTION('center_axis',(0.,-1.,0.));
#19489=DIRECTION('ref_axis',(6.12323399573677E-17,0.,-1.));
#19490=DIRECTION('center_axis',(0.,1.,0.));
#19491=DIRECTION('ref_axis',(1.,0.,0.));
#19492=DIRECTION('center_axis',(0.,-1.,0.));
#19493=DIRECTION('ref_axis',(-0.309016994374947,0.,-0.951056516295154));
#19494=DIRECTION('center_axis',(0.,1.,0.));
#19495=DIRECTION('ref_axis',(1.,0.,0.));
#19496=DIRECTION('center_axis',(0.,-1.,0.));
#19497=DIRECTION('ref_axis',(-0.587785252292473,0.,-0.809016994374948));
#19498=DIRECTION('center_axis',(0.,1.,0.));
#19499=DIRECTION('ref_axis',(1.,0.,0.));
#19500=DIRECTION('center_axis',(0.,-1.,0.));
#19501=DIRECTION('ref_axis',(-0.809016994374947,0.,-0.587785252292473));
#19502=DIRECTION('center_axis',(0.,1.,0.));
#19503=DIRECTION('ref_axis',(1.,0.,0.));
#19504=DIRECTION('center_axis',(0.,-1.,0.));
#19505=DIRECTION('ref_axis',(-0.951056516295154,0.,-0.309016994374948));
#19506=DIRECTION('center_axis',(0.,1.,0.));
#19507=DIRECTION('ref_axis',(1.,0.,0.));
#19508=DIRECTION('center_axis',(0.,-1.,0.));
#19509=DIRECTION('ref_axis',(-1.,0.,-1.22464679914735E-16));
#19510=DIRECTION('center_axis',(0.,1.,0.));
#19511=DIRECTION('ref_axis',(1.,0.,0.));
#19512=DIRECTION('center_axis',(0.,-1.,0.));
#19513=DIRECTION('ref_axis',(-0.951056516295154,0.,0.309016994374947));
#19514=DIRECTION('center_axis',(0.,1.,0.));
#19515=DIRECTION('ref_axis',(1.,0.,0.));
#19516=DIRECTION('center_axis',(0.,-1.,0.));
#19517=DIRECTION('ref_axis',(-0.809016994374947,0.,0.587785252292473));
#19518=DIRECTION('center_axis',(0.,1.,0.));
#19519=DIRECTION('ref_axis',(1.,0.,0.));
#19520=DIRECTION('center_axis',(0.,-1.,0.));
#19521=DIRECTION('ref_axis',(-0.587785252292473,0.,0.809016994374947));
#19522=DIRECTION('center_axis',(0.,1.,0.));
#19523=DIRECTION('ref_axis',(1.,0.,0.));
#19524=DIRECTION('center_axis',(0.,-1.,0.));
#19525=DIRECTION('ref_axis',(-0.309016994374948,0.,0.951056516295154));
#19526=DIRECTION('center_axis',(0.,1.,0.));
#19527=DIRECTION('ref_axis',(1.,0.,0.));
#19528=DIRECTION('center_axis',(0.,-1.,0.));
#19529=DIRECTION('ref_axis',(-1.83697019872103E-16,0.,1.));
#19530=DIRECTION('center_axis',(0.,1.,0.));
#19531=DIRECTION('ref_axis',(1.,0.,0.));
#19532=DIRECTION('center_axis',(0.,-1.,0.));
#19533=DIRECTION('ref_axis',(0.309016994374947,0.,0.951056516295154));
#19534=DIRECTION('center_axis',(0.,1.,0.));
#19535=DIRECTION('ref_axis',(1.,0.,0.));
#19536=DIRECTION('center_axis',(0.,-1.,0.));
#19537=DIRECTION('ref_axis',(0.587785252292473,0.,0.809016994374948));
#19538=DIRECTION('center_axis',(0.,1.,0.));
#19539=DIRECTION('ref_axis',(1.,0.,0.));
#19540=DIRECTION('center_axis',(0.,-1.,0.));
#19541=DIRECTION('ref_axis',(0.809016994374947,0.,0.587785252292473));
#19542=DIRECTION('center_axis',(0.,1.,0.));
#19543=DIRECTION('ref_axis',(1.,0.,0.));
#19544=DIRECTION('center_axis',(0.,1.,0.));
#19545=DIRECTION('ref_axis',(1.,0.,0.));
#19546=DIRECTION('center_axis',(0.,1.,0.));
#19547=DIRECTION('ref_axis',(1.,0.,0.));
#19548=DIRECTION('',(0.,-1.,0.));
#19549=DIRECTION('center_axis',(0.,1.,0.));
#19550=DIRECTION('ref_axis',(1.,0.,0.));
#19551=DIRECTION('center_axis',(0.,1.,0.));
#19552=DIRECTION('ref_axis',(-0.951056516295153,0.,-0.309016994374948));
#19553=DIRECTION('',(0.,-1.,0.));
#19554=DIRECTION('',(0.,1.,0.));
#19555=DIRECTION('center_axis',(0.,1.,0.));
#19556=DIRECTION('ref_axis',(1.,0.,0.));
#19557=DIRECTION('',(0.,-1.,0.));
#19558=DIRECTION('center_axis',(0.,1.,0.));
#19559=DIRECTION('ref_axis',(-0.809016994374947,0.,-0.587785252292473));
#19560=DIRECTION('',(0.,1.,0.));
#19561=DIRECTION('center_axis',(0.,1.,0.));
#19562=DIRECTION('ref_axis',(1.,0.,0.));
#19563=DIRECTION('',(0.,-1.,0.));
#19564=DIRECTION('center_axis',(0.,1.,0.));
#19565=DIRECTION('ref_axis',(-0.587785252292473,0.,-0.809016994374947));
#19566=DIRECTION('',(0.,1.,0.));
#19567=DIRECTION('center_axis',(0.,1.,0.));
#19568=DIRECTION('ref_axis',(1.,0.,0.));
#19569=DIRECTION('',(0.,-1.,0.));
#19570=DIRECTION('center_axis',(0.,1.,0.));
#19571=DIRECTION('ref_axis',(-0.309016994374947,0.,-0.951056516295154));
#19572=DIRECTION('',(0.,1.,0.));
#19573=DIRECTION('center_axis',(0.,1.,0.));
#19574=DIRECTION('ref_axis',(1.,0.,0.));
#19575=DIRECTION('',(0.,-1.,0.));
#19576=DIRECTION('center_axis',(0.,1.,0.));
#19577=DIRECTION('ref_axis',(-1.37927510063224E-16,0.,-1.));
#19578=DIRECTION('',(0.,1.,0.));
#19579=DIRECTION('center_axis',(0.,1.,0.));
#19580=DIRECTION('ref_axis',(1.,0.,0.));
#19581=DIRECTION('',(0.,-1.,0.));
#19582=DIRECTION('center_axis',(0.,1.,0.));
#19583=DIRECTION('ref_axis',(0.309016994374948,0.,-0.951056516295154));
#19584=DIRECTION('',(0.,1.,0.));
#19585=DIRECTION('center_axis',(0.,1.,0.));
#19586=DIRECTION('ref_axis',(1.,0.,0.));
#19587=DIRECTION('',(0.,-1.,0.));
#19588=DIRECTION('center_axis',(0.,1.,0.));
#19589=DIRECTION('ref_axis',(0.587785252292473,0.,-0.809016994374948));
#19590=DIRECTION('',(0.,1.,0.));
#19591=DIRECTION('center_axis',(0.,1.,0.));
#19592=DIRECTION('ref_axis',(1.,0.,0.));
#19593=DIRECTION('',(0.,-1.,0.));
#19594=DIRECTION('center_axis',(0.,1.,0.));
#19595=DIRECTION('ref_axis',(0.809016994374948,0.,-0.587785252292473));
#19596=DIRECTION('',(0.,1.,0.));
#19597=DIRECTION('center_axis',(0.,1.,0.));
#19598=DIRECTION('ref_axis',(1.,0.,0.));
#19599=DIRECTION('',(0.,-1.,0.));
#19600=DIRECTION('center_axis',(0.,1.,0.));
#19601=DIRECTION('ref_axis',(0.951056516295154,0.,-0.309016994374947));
#19602=DIRECTION('',(0.,1.,0.));
#19603=DIRECTION('center_axis',(0.,1.,0.));
#19604=DIRECTION('ref_axis',(1.,0.,0.));
#19605=DIRECTION('',(0.,-1.,0.));
#19606=DIRECTION('center_axis',(0.,1.,0.));
#19607=DIRECTION('ref_axis',(1.,0.,-1.99159850020592E-16));
#19608=DIRECTION('',(0.,1.,0.));
#19609=DIRECTION('center_axis',(0.,1.,0.));
#19610=DIRECTION('ref_axis',(1.,0.,0.));
#19611=DIRECTION('',(0.,-1.,0.));
#19612=DIRECTION('center_axis',(0.,1.,0.));
#19613=DIRECTION('ref_axis',(0.951056516295154,0.,0.309016994374948));
#19614=DIRECTION('',(0.,1.,0.));
#19615=DIRECTION('center_axis',(0.,1.,0.));
#19616=DIRECTION('ref_axis',(1.,0.,0.));
#19617=DIRECTION('',(0.,-1.,0.));
#19618=DIRECTION('center_axis',(0.,1.,0.));
#19619=DIRECTION('ref_axis',(0.809016994374948,0.,0.587785252292473));
#19620=DIRECTION('',(0.,1.,0.));
#19621=DIRECTION('center_axis',(0.,1.,0.));
#19622=DIRECTION('ref_axis',(1.,0.,0.));
#19623=DIRECTION('',(0.,-1.,0.));
#19624=DIRECTION('center_axis',(0.,1.,0.));
#19625=DIRECTION('ref_axis',(0.587785252292473,0.,0.809016994374948));
#19626=DIRECTION('',(0.,1.,0.));
#19627=DIRECTION('center_axis',(0.,1.,0.));
#19628=DIRECTION('ref_axis',(1.,0.,0.));
#19629=DIRECTION('',(0.,-1.,0.));
#19630=DIRECTION('center_axis',(0.,1.,0.));
#19631=DIRECTION('ref_axis',(0.309016994374947,0.,0.951056516295154));
#19632=DIRECTION('',(0.,1.,0.));
#19633=DIRECTION('center_axis',(0.,1.,0.));
#19634=DIRECTION('ref_axis',(1.,0.,0.));
#19635=DIRECTION('',(0.,-1.,0.));
#19636=DIRECTION('center_axis',(0.,1.,0.));
#19637=DIRECTION('ref_axis',(2.6039218997796E-16,0.,1.));
#19638=DIRECTION('',(0.,1.,0.));
#19639=DIRECTION('center_axis',(0.,1.,0.));
#19640=DIRECTION('ref_axis',(1.,0.,0.));
#19641=DIRECTION('',(0.,-1.,0.));
#19642=DIRECTION('center_axis',(0.,1.,0.));
#19643=DIRECTION('ref_axis',(-0.309016994374948,0.,0.951056516295153));
#19644=DIRECTION('',(0.,1.,0.));
#19645=DIRECTION('center_axis',(0.,1.,0.));
#19646=DIRECTION('ref_axis',(1.,0.,0.));
#19647=DIRECTION('',(0.,-1.,0.));
#19648=DIRECTION('center_axis',(0.,1.,0.));
#19649=DIRECTION('ref_axis',(-0.587785252292474,0.,0.809016994374947));
#19650=DIRECTION('',(0.,1.,0.));
#19651=DIRECTION('center_axis',(0.,1.,0.));
#19652=DIRECTION('ref_axis',(1.,0.,0.));
#19653=DIRECTION('',(0.,-1.,0.));
#19654=DIRECTION('center_axis',(0.,1.,0.));
#19655=DIRECTION('ref_axis',(-0.809016994374948,0.,0.587785252292473));
#19656=DIRECTION('',(0.,1.,0.));
#19657=DIRECTION('center_axis',(0.,1.,0.));
#19658=DIRECTION('ref_axis',(1.,0.,0.));
#19659=DIRECTION('',(0.,-1.,0.));
#19660=DIRECTION('center_axis',(0.,1.,0.));
#19661=DIRECTION('ref_axis',(-0.951056516295154,0.,0.309016994374948));
#19662=DIRECTION('',(0.,1.,0.));
#19663=DIRECTION('center_axis',(0.,1.,0.));
#19664=DIRECTION('ref_axis',(1.,0.,0.));
#19665=DIRECTION('',(0.,1.,0.));
#19666=DIRECTION('center_axis',(0.,1.,0.));
#19667=DIRECTION('ref_axis',(-1.,0.,-1.22464679914735E-16));
#19668=DIRECTION('',(0.,-1.,0.));
#19669=DIRECTION('center_axis',(0.,1.,0.));
#19670=DIRECTION('ref_axis',(1.,0.,0.));
#19671=DIRECTION('axis',(0.,0.,1.));
#19672=DIRECTION('refdir',(1.,0.,0.));
#19673=DIRECTION('axis',(0.,0.,1.));
#19674=DIRECTION('refdir',(1.,0.,0.));
#19675=DIRECTION('center_axis',(0.,1.,0.));
#19676=DIRECTION('ref_axis',(1.,0.,0.));
#19677=DIRECTION('center_axis',(0.,1.,0.));
#19678=DIRECTION('ref_axis',(1.,0.,0.));
#19679=DIRECTION('center_axis',(0.,1.,0.));
#19680=DIRECTION('ref_axis',(1.,0.,0.));
#19681=DIRECTION('center_axis',(0.,1.,0.));
#19682=DIRECTION('ref_axis',(1.,0.,0.));
#19683=DIRECTION('center_axis',(0.,1.,0.));
#19684=DIRECTION('ref_axis',(1.,0.,0.));
#19685=DIRECTION('',(0.,-1.,0.));
#19686=DIRECTION('center_axis',(0.,1.,0.));
#19687=DIRECTION('ref_axis',(1.,0.,0.));
#19688=DIRECTION('center_axis',(0.,1.,0.));
#19689=DIRECTION('ref_axis',(1.,0.,0.));
#19690=DIRECTION('center_axis',(0.,1.,0.));
#19691=DIRECTION('ref_axis',(1.,0.,0.));
#19692=DIRECTION('',(0.,1.,0.));
#19693=DIRECTION('center_axis',(0.,1.,0.));
#19694=DIRECTION('ref_axis',(1.,0.,0.));
#19695=DIRECTION('center_axis',(0.,1.,0.));
#19696=DIRECTION('ref_axis',(1.,0.,0.));
#19697=DIRECTION('center_axis',(0.,1.,0.));
#19698=DIRECTION('ref_axis',(1.,0.,0.));
#19699=DIRECTION('center_axis',(0.,1.,0.));
#19700=DIRECTION('ref_axis',(1.,0.,0.));
#19701=DIRECTION('center_axis',(0.,-1.,0.));
#19702=DIRECTION('ref_axis',(1.,0.,0.));
#19703=DIRECTION('center_axis',(0.,1.,0.));
#19704=DIRECTION('ref_axis',(1.,0.,0.));
#19705=DIRECTION('',(0.,-1.,0.));
#19706=DIRECTION('center_axis',(0.,1.,0.));
#19707=DIRECTION('ref_axis',(1.,0.,0.));
#19708=DIRECTION('',(0.,-1.,0.));
#19709=DIRECTION('center_axis',(0.,1.,0.));
#19710=DIRECTION('ref_axis',(1.,0.,0.));
#19711=DIRECTION('center_axis',(0.,1.,0.));
#19712=DIRECTION('ref_axis',(1.,0.,0.));
#19713=DIRECTION('axis',(0.,0.,1.));
#19714=DIRECTION('refdir',(1.,0.,0.));
#19715=DIRECTION('center_axis',(0.,1.,0.));
#19716=DIRECTION('ref_axis',(1.,0.,0.));
#19717=DIRECTION('center_axis',(0.,-1.,0.));
#19718=DIRECTION('ref_axis',(1.,0.,0.));
#19719=DIRECTION('',(0.,-1.,0.));
#19720=DIRECTION('center_axis',(0.,-1.,0.));
#19721=DIRECTION('ref_axis',(1.,0.,0.));
#19722=DIRECTION('center_axis',(0.,1.,0.));
#19723=DIRECTION('ref_axis',(1.,0.,0.));
#19724=DIRECTION('center_axis',(0.,1.,0.));
#19725=DIRECTION('ref_axis',(1.,0.,0.));
#19726=DIRECTION('',(0.,-1.,0.));
#19727=DIRECTION('center_axis',(0.,1.,0.));
#19728=DIRECTION('ref_axis',(1.,0.,0.));
#19729=DIRECTION('center_axis',(0.,1.,0.));
#19730=DIRECTION('ref_axis',(1.,0.,0.));
#19731=DIRECTION('center_axis',(0.,1.,0.));
#19732=DIRECTION('ref_axis',(1.,0.,0.));
#19733=DIRECTION('axis',(0.,0.,1.));
#19734=DIRECTION('refdir',(1.,0.,0.));
#19735=DIRECTION('center_axis',(0.,1.,0.));
#19736=DIRECTION('ref_axis',(1.,0.,0.));
#19737=DIRECTION('center_axis',(0.,-1.,0.));
#19738=DIRECTION('ref_axis',(1.,0.,0.));
#19739=DIRECTION('',(0.,-1.,0.));
#19740=DIRECTION('center_axis',(0.,-1.,0.));
#19741=DIRECTION('ref_axis',(1.,0.,0.));
#19742=DIRECTION('center_axis',(0.,1.,0.));
#19743=DIRECTION('ref_axis',(1.,0.,0.));
#19744=DIRECTION('center_axis',(0.,1.,0.));
#19745=DIRECTION('ref_axis',(1.,0.,0.));
#19746=DIRECTION('',(0.,-1.,0.));
#19747=DIRECTION('center_axis',(0.,1.,0.));
#19748=DIRECTION('ref_axis',(1.,0.,0.));
#19749=DIRECTION('center_axis',(0.,1.,0.));
#19750=DIRECTION('ref_axis',(1.,0.,0.));
#19751=DIRECTION('center_axis',(0.,1.,0.));
#19752=DIRECTION('ref_axis',(1.,0.,0.));
#19753=DIRECTION('axis',(0.,0.,1.));
#19754=DIRECTION('refdir',(1.,0.,0.));
#19755=DIRECTION('center_axis',(0.,0.,1.));
#19756=DIRECTION('ref_axis',(1.,0.,0.));
#19757=DIRECTION('center_axis',(0.,0.,1.));
#19758=DIRECTION('ref_axis',(1.,0.,0.));
#19759=DIRECTION('',(0.,0.,-1.));
#19760=DIRECTION('center_axis',(0.,0.,1.));
#19761=DIRECTION('ref_axis',(1.,0.,0.));
#19762=DIRECTION('center_axis',(0.,0.,1.));
#19763=DIRECTION('ref_axis',(1.,0.,0.));
#19764=DIRECTION('center_axis',(0.,0.,1.));
#19765=DIRECTION('ref_axis',(1.,0.,0.));
#19766=DIRECTION('axis',(0.,0.,1.));
#19767=DIRECTION('refdir',(1.,0.,0.));
#19768=DIRECTION('center_axis',(0.,0.,1.));
#19769=DIRECTION('ref_axis',(1.,0.,0.));
#19770=DIRECTION('center_axis',(0.,0.,1.));
#19771=DIRECTION('ref_axis',(1.,0.,0.));
#19772=DIRECTION('',(0.,0.,-1.));
#19773=DIRECTION('center_axis',(0.,0.,1.));
#19774=DIRECTION('ref_axis',(1.,0.,0.));
#19775=DIRECTION('center_axis',(0.,0.,1.));
#19776=DIRECTION('ref_axis',(1.,0.,0.));
#19777=DIRECTION('center_axis',(0.,0.,1.));
#19778=DIRECTION('ref_axis',(1.,0.,0.));
#19779=DIRECTION('axis',(0.,0.,1.));
#19780=DIRECTION('refdir',(1.,0.,0.));
#19781=DIRECTION('center_axis',(0.,1.,0.));
#19782=DIRECTION('ref_axis',(1.,0.,0.));
#19783=DIRECTION('center_axis',(0.,-1.,0.));
#19784=DIRECTION('ref_axis',(1.,0.,0.));
#19785=DIRECTION('',(0.,-1.,0.));
#19786=DIRECTION('center_axis',(0.,-1.,0.));
#19787=DIRECTION('ref_axis',(1.,0.,0.));
#19788=DIRECTION('center_axis',(0.,1.,0.));
#19789=DIRECTION('ref_axis',(1.,0.,0.));
#19790=DIRECTION('center_axis',(0.,1.,0.));
#19791=DIRECTION('ref_axis',(1.,0.,0.));
#19792=DIRECTION('',(0.,-1.,0.));
#19793=DIRECTION('center_axis',(0.,1.,0.));
#19794=DIRECTION('ref_axis',(1.,0.,0.));
#19795=DIRECTION('center_axis',(0.,1.,0.));
#19796=DIRECTION('ref_axis',(1.,0.,0.));
#19797=DIRECTION('center_axis',(0.,1.,0.));
#19798=DIRECTION('ref_axis',(1.,0.,0.));
#19799=DIRECTION('axis',(0.,0.,1.));
#19800=DIRECTION('refdir',(1.,0.,0.));
#19801=DIRECTION('center_axis',(0.,0.,1.));
#19802=DIRECTION('ref_axis',(1.,0.,0.));
#19803=DIRECTION('',(0.,1.,0.));
#19804=DIRECTION('center_axis',(0.,0.,1.));
#19805=DIRECTION('ref_axis',(1.,0.,0.));
#19806=DIRECTION('center_axis',(0.,0.,1.));
#19807=DIRECTION('ref_axis',(1.,0.,0.));
#19808=DIRECTION('center_axis',(0.,0.,1.));
#19809=DIRECTION('ref_axis',(1.,0.,0.));
#19810=DIRECTION('',(0.,0.,1.));
#19811=DIRECTION('center_axis',(0.,0.,1.));
#19812=DIRECTION('ref_axis',(1.,0.,0.));
#19813=DIRECTION('center_axis',(0.,0.,1.));
#19814=DIRECTION('ref_axis',(1.,0.,0.));
#19815=DIRECTION('',(0.,-1.,0.));
#19816=DIRECTION('center_axis',(0.,1.,0.));
#19817=DIRECTION('ref_axis',(1.,0.,0.));
#19818=DIRECTION('center_axis',(0.,-1.,0.));
#19819=DIRECTION('ref_axis',(1.,0.,0.));
#19820=DIRECTION('',(0.,-1.,0.));
#19821=DIRECTION('center_axis',(0.,-1.,0.));
#19822=DIRECTION('ref_axis',(1.,0.,0.));
#19823=DIRECTION('center_axis',(0.,1.,0.));
#19824=DIRECTION('ref_axis',(1.,0.,0.));
#19825=DIRECTION('center_axis',(0.,1.,0.));
#19826=DIRECTION('ref_axis',(1.,0.,0.));
#19827=DIRECTION('',(0.,-1.,0.));
#19828=DIRECTION('center_axis',(0.,1.,0.));
#19829=DIRECTION('ref_axis',(1.,0.,0.));
#19830=DIRECTION('center_axis',(0.,1.,0.));
#19831=DIRECTION('ref_axis',(1.,0.,0.));
#19832=DIRECTION('center_axis',(0.,1.,0.));
#19833=DIRECTION('ref_axis',(1.,0.,0.));
#19834=DIRECTION('axis',(0.,0.,1.));
#19835=DIRECTION('refdir',(1.,0.,0.));
#19836=DIRECTION('center_axis',(0.,0.,1.));
#19837=DIRECTION('ref_axis',(1.,0.,0.));
#19838=DIRECTION('',(0.,1.,0.));
#19839=DIRECTION('center_axis',(0.,0.,1.));
#19840=DIRECTION('ref_axis',(1.,0.,0.));
#19841=DIRECTION('center_axis',(0.,0.,1.));
#19842=DIRECTION('ref_axis',(1.,0.,0.));
#19843=DIRECTION('center_axis',(0.,0.,1.));
#19844=DIRECTION('ref_axis',(1.,0.,0.));
#19845=DIRECTION('',(0.,0.,1.));
#19846=DIRECTION('center_axis',(0.,0.,1.));
#19847=DIRECTION('ref_axis',(1.,0.,0.));
#19848=DIRECTION('center_axis',(0.,0.,1.));
#19849=DIRECTION('ref_axis',(1.,0.,0.));
#19850=DIRECTION('',(0.,-1.,0.));
#19851=DIRECTION('center_axis',(0.,1.,0.));
#19852=DIRECTION('ref_axis',(1.,0.,0.));
#19853=DIRECTION('center_axis',(0.,-1.,0.));
#19854=DIRECTION('ref_axis',(1.,0.,0.));
#19855=DIRECTION('',(0.,-1.,0.));
#19856=DIRECTION('center_axis',(0.,-1.,0.));
#19857=DIRECTION('ref_axis',(1.,0.,0.));
#19858=DIRECTION('center_axis',(0.,1.,0.));
#19859=DIRECTION('ref_axis',(1.,0.,0.));
#19860=DIRECTION('center_axis',(0.,1.,0.));
#19861=DIRECTION('ref_axis',(1.,0.,0.));
#19862=DIRECTION('',(0.,-1.,0.));
#19863=DIRECTION('center_axis',(0.,1.,0.));
#19864=DIRECTION('ref_axis',(1.,0.,0.));
#19865=DIRECTION('center_axis',(0.,1.,0.));
#19866=DIRECTION('ref_axis',(1.,0.,0.));
#19867=DIRECTION('center_axis',(0.,1.,0.));
#19868=DIRECTION('ref_axis',(1.,0.,0.));
#19869=DIRECTION('axis',(0.,0.,1.));
#19870=DIRECTION('refdir',(1.,0.,0.));
#19871=DIRECTION('center_axis',(0.,1.,0.));
#19872=DIRECTION('ref_axis',(1.,0.,0.));
#19873=DIRECTION('center_axis',(0.,-1.,0.));
#19874=DIRECTION('ref_axis',(1.,0.,0.));
#19875=DIRECTION('',(0.,-1.,0.));
#19876=DIRECTION('center_axis',(0.,-1.,0.));
#19877=DIRECTION('ref_axis',(1.,0.,0.));
#19878=DIRECTION('center_axis',(0.,1.,0.));
#19879=DIRECTION('ref_axis',(1.,0.,0.));
#19880=DIRECTION('center_axis',(0.,1.,0.));
#19881=DIRECTION('ref_axis',(1.,0.,0.));
#19882=DIRECTION('',(0.,-1.,0.));
#19883=DIRECTION('center_axis',(0.,1.,0.));
#19884=DIRECTION('ref_axis',(1.,0.,0.));
#19885=DIRECTION('center_axis',(0.,1.,0.));
#19886=DIRECTION('ref_axis',(1.,0.,0.));
#19887=DIRECTION('center_axis',(0.,1.,0.));
#19888=DIRECTION('ref_axis',(1.,0.,0.));
#19889=DIRECTION('axis',(0.,0.,1.));
#19890=DIRECTION('refdir',(1.,0.,0.));
#19891=DIRECTION('center_axis',(0.,1.,0.));
#19892=DIRECTION('ref_axis',(1.,0.,0.));
#19893=DIRECTION('center_axis',(0.,-1.,0.));
#19894=DIRECTION('ref_axis',(1.,0.,0.));
#19895=DIRECTION('',(0.,-1.,0.));
#19896=DIRECTION('center_axis',(0.,-1.,0.));
#19897=DIRECTION('ref_axis',(1.,0.,0.));
#19898=DIRECTION('center_axis',(0.,1.,0.));
#19899=DIRECTION('ref_axis',(1.,0.,0.));
#19900=DIRECTION('center_axis',(0.,1.,0.));
#19901=DIRECTION('ref_axis',(1.,0.,0.));
#19902=DIRECTION('',(0.,-1.,0.));
#19903=DIRECTION('center_axis',(0.,1.,0.));
#19904=DIRECTION('ref_axis',(1.,0.,0.));
#19905=DIRECTION('center_axis',(0.,1.,0.));
#19906=DIRECTION('ref_axis',(1.,0.,0.));
#19907=DIRECTION('center_axis',(0.,1.,0.));
#19908=DIRECTION('ref_axis',(1.,0.,0.));
#19909=DIRECTION('axis',(0.,0.,1.));
#19910=DIRECTION('refdir',(1.,0.,0.));
#19911=DIRECTION('center_axis',(0.,1.,0.));
#19912=DIRECTION('ref_axis',(1.,0.,0.));
#19913=DIRECTION('center_axis',(0.,-1.,0.));
#19914=DIRECTION('ref_axis',(1.,0.,0.));
#19915=DIRECTION('',(0.,-1.,0.));
#19916=DIRECTION('center_axis',(0.,-1.,0.));
#19917=DIRECTION('ref_axis',(1.,0.,0.));
#19918=DIRECTION('center_axis',(0.,1.,0.));
#19919=DIRECTION('ref_axis',(1.,0.,0.));
#19920=DIRECTION('center_axis',(0.,1.,0.));
#19921=DIRECTION('ref_axis',(1.,0.,0.));
#19922=DIRECTION('',(0.,-1.,0.));
#19923=DIRECTION('center_axis',(0.,1.,0.));
#19924=DIRECTION('ref_axis',(1.,0.,0.));
#19925=DIRECTION('center_axis',(0.,1.,0.));
#19926=DIRECTION('ref_axis',(1.,0.,0.));
#19927=DIRECTION('center_axis',(0.,1.,0.));
#19928=DIRECTION('ref_axis',(1.,0.,0.));
#19929=DIRECTION('axis',(0.,0.,1.));
#19930=DIRECTION('refdir',(1.,0.,0.));
#19931=DIRECTION('center_axis',(0.,0.,1.));
#19932=DIRECTION('ref_axis',(1.,0.,0.));
#19933=DIRECTION('',(0.,1.,0.));
#19934=DIRECTION('center_axis',(0.,0.,1.));
#19935=DIRECTION('ref_axis',(1.,0.,0.));
#19936=DIRECTION('center_axis',(0.,0.,1.));
#19937=DIRECTION('ref_axis',(1.,0.,0.));
#19938=DIRECTION('center_axis',(0.,0.,1.));
#19939=DIRECTION('ref_axis',(1.,0.,0.));
#19940=DIRECTION('',(0.,0.,1.));
#19941=DIRECTION('center_axis',(0.,0.,1.));
#19942=DIRECTION('ref_axis',(1.,0.,0.));
#19943=DIRECTION('center_axis',(0.,0.,1.));
#19944=DIRECTION('ref_axis',(1.,0.,0.));
#19945=DIRECTION('',(0.,-1.,0.));
#19946=DIRECTION('center_axis',(0.,1.,0.));
#19947=DIRECTION('ref_axis',(1.,0.,0.));
#19948=DIRECTION('center_axis',(0.,-1.,0.));
#19949=DIRECTION('ref_axis',(1.,0.,0.));
#19950=DIRECTION('',(0.,-1.,0.));
#19951=DIRECTION('center_axis',(0.,-1.,0.));
#19952=DIRECTION('ref_axis',(1.,0.,0.));
#19953=DIRECTION('center_axis',(0.,1.,0.));
#19954=DIRECTION('ref_axis',(1.,0.,0.));
#19955=DIRECTION('center_axis',(0.,1.,0.));
#19956=DIRECTION('ref_axis',(1.,0.,0.));
#19957=DIRECTION('',(0.,-1.,0.));
#19958=DIRECTION('center_axis',(0.,1.,0.));
#19959=DIRECTION('ref_axis',(1.,0.,0.));
#19960=DIRECTION('center_axis',(0.,1.,0.));
#19961=DIRECTION('ref_axis',(1.,0.,0.));
#19962=DIRECTION('center_axis',(0.,1.,0.));
#19963=DIRECTION('ref_axis',(1.,0.,0.));
#19964=DIRECTION('axis',(0.,0.,1.));
#19965=DIRECTION('refdir',(1.,0.,0.));
#19966=DIRECTION('center_axis',(0.,0.,1.));
#19967=DIRECTION('ref_axis',(1.,0.,0.));
#19968=DIRECTION('',(0.,1.,0.));
#19969=DIRECTION('center_axis',(0.,0.,1.));
#19970=DIRECTION('ref_axis',(1.,0.,0.));
#19971=DIRECTION('center_axis',(0.,0.,1.));
#19972=DIRECTION('ref_axis',(1.,0.,0.));
#19973=DIRECTION('center_axis',(0.,0.,1.));
#19974=DIRECTION('ref_axis',(1.,0.,0.));
#19975=DIRECTION('',(0.,0.,1.));
#19976=DIRECTION('center_axis',(0.,0.,1.));
#19977=DIRECTION('ref_axis',(1.,0.,0.));
#19978=DIRECTION('center_axis',(0.,0.,1.));
#19979=DIRECTION('ref_axis',(1.,0.,0.));
#19980=DIRECTION('',(0.,-1.,0.));
#19981=DIRECTION('center_axis',(0.,1.,0.));
#19982=DIRECTION('ref_axis',(1.,0.,0.));
#19983=DIRECTION('center_axis',(0.,-1.,0.));
#19984=DIRECTION('ref_axis',(1.,0.,0.));
#19985=DIRECTION('',(0.,-1.,0.));
#19986=DIRECTION('center_axis',(0.,-1.,0.));
#19987=DIRECTION('ref_axis',(1.,0.,0.));
#19988=DIRECTION('center_axis',(0.,1.,0.));
#19989=DIRECTION('ref_axis',(1.,0.,0.));
#19990=DIRECTION('center_axis',(0.,1.,0.));
#19991=DIRECTION('ref_axis',(1.,0.,0.));
#19992=DIRECTION('',(0.,-1.,0.));
#19993=DIRECTION('center_axis',(0.,1.,0.));
#19994=DIRECTION('ref_axis',(1.,0.,0.));
#19995=DIRECTION('center_axis',(0.,1.,0.));
#19996=DIRECTION('ref_axis',(1.,0.,0.));
#19997=DIRECTION('center_axis',(0.,1.,0.));
#19998=DIRECTION('ref_axis',(1.,0.,0.));
#19999=DIRECTION('axis',(0.,0.,1.));
#20000=DIRECTION('refdir',(1.,0.,0.));
#20001=DIRECTION('center_axis',(1.,0.,6.12323399573677E-17));
#20002=DIRECTION('ref_axis',(6.12323399573677E-17,0.,-1.));
#20003=DIRECTION('',(1.,0.,6.12323399573677E-17));
#20004=DIRECTION('center_axis',(1.,0.,6.12323399573677E-17));
#20005=DIRECTION('ref_axis',(6.12323399573677E-17,0.,-1.));
#20006=DIRECTION('',(1.,0.,6.12323399573677E-17));
#20007=DIRECTION('center_axis',(0.,-1.,0.));
#20008=DIRECTION('ref_axis',(1.,0.,0.));
#20009=DIRECTION('center_axis',(0.,-1.,0.));
#20010=DIRECTION('ref_axis',(1.,0.,0.));
#20011=DIRECTION('',(0.,1.,0.));
#20012=DIRECTION('',(0.,1.,0.));
#20013=DIRECTION('center_axis',(0.,1.,0.));
#20014=DIRECTION('ref_axis',(1.,0.,0.));
#20015=DIRECTION('center_axis',(0.,0.,1.));
#20016=DIRECTION('ref_axis',(1.,0.,0.));
#20017=DIRECTION('',(0.,0.,1.));
#20018=DIRECTION('center_axis',(0.,0.,1.));
#20019=DIRECTION('ref_axis',(1.,0.,0.));
#20020=DIRECTION('',(0.,0.,1.));
#20021=DIRECTION('center_axis',(0.,1.,0.));
#20022=DIRECTION('ref_axis',(1.,0.,0.));
#20023=DIRECTION('center_axis',(0.,1.,0.));
#20024=DIRECTION('ref_axis',(1.,0.,0.));
#20025=DIRECTION('',(0.,1.,0.));
#20026=DIRECTION('',(0.,1.,0.));
#20027=DIRECTION('center_axis',(0.,-1.,0.));
#20028=DIRECTION('ref_axis',(1.,0.,0.));
#20029=DIRECTION('center_axis',(0.,1.,0.));
#20030=DIRECTION('ref_axis',(1.,0.,0.));
#20031=DIRECTION('center_axis',(0.,1.,0.));
#20032=DIRECTION('ref_axis',(1.,0.,0.));
#20033=DIRECTION('center_axis',(0.,1.,0.));
#20034=DIRECTION('ref_axis',(1.,0.,0.));
#20035=DIRECTION('center_axis',(0.,1.,0.));
#20036=DIRECTION('ref_axis',(0.987688340595138,0.,0.156434465040231));
#20037=DIRECTION('center_axis',(0.,1.,0.));
#20038=DIRECTION('ref_axis',(1.,0.,0.));
#20039=DIRECTION('center_axis',(0.,1.,0.));
#20040=DIRECTION('ref_axis',(0.951056516295154,0.,0.309016994374948));
#20041=DIRECTION('center_axis',(0.,1.,0.));
#20042=DIRECTION('ref_axis',(1.,0.,0.));
#20043=DIRECTION('center_axis',(0.,1.,0.));
#20044=DIRECTION('ref_axis',(0.891006524188368,0.,0.453990499739547));
#20045=DIRECTION('center_axis',(0.,1.,0.));
#20046=DIRECTION('ref_axis',(1.,0.,0.));
#20047=DIRECTION('center_axis',(0.,1.,0.));
#20048=DIRECTION('ref_axis',(0.809016994374947,0.,0.587785252292473));
#20049=DIRECTION('center_axis',(0.,1.,0.));
#20050=DIRECTION('ref_axis',(1.,0.,0.));
#20051=DIRECTION('center_axis',(0.,1.,0.));
#20052=DIRECTION('ref_axis',(0.707106781186547,0.,0.707106781186548));
#20053=DIRECTION('center_axis',(0.,1.,0.));
#20054=DIRECTION('ref_axis',(1.,0.,0.));
#20055=DIRECTION('center_axis',(0.,1.,0.));
#20056=DIRECTION('ref_axis',(0.587785252292473,0.,0.809016994374948));
#20057=DIRECTION('center_axis',(0.,1.,0.));
#20058=DIRECTION('ref_axis',(1.,0.,0.));
#20059=DIRECTION('center_axis',(0.,1.,0.));
#20060=DIRECTION('ref_axis',(0.453990499739547,0.,0.891006524188368));
#20061=DIRECTION('center_axis',(0.,1.,0.));
#20062=DIRECTION('ref_axis',(1.,0.,0.));
#20063=DIRECTION('center_axis',(0.,1.,0.));
#20064=DIRECTION('ref_axis',(0.309016994374947,0.,0.951056516295154));
#20065=DIRECTION('center_axis',(0.,1.,0.));
#20066=DIRECTION('ref_axis',(1.,0.,0.));
#20067=DIRECTION('center_axis',(0.,1.,0.));
#20068=DIRECTION('ref_axis',(0.156434465040231,0.,0.987688340595138));
#20069=DIRECTION('center_axis',(0.,1.,0.));
#20070=DIRECTION('ref_axis',(1.,0.,0.));
#20071=DIRECTION('center_axis',(0.,1.,0.));
#20072=DIRECTION('ref_axis',(-1.83697019872103E-16,0.,1.));
#20073=DIRECTION('center_axis',(0.,1.,0.));
#20074=DIRECTION('ref_axis',(1.,0.,0.));
#20075=DIRECTION('center_axis',(0.,1.,0.));
#20076=DIRECTION('ref_axis',(-0.156434465040231,0.,0.987688340595138));
#20077=DIRECTION('center_axis',(0.,1.,0.));
#20078=DIRECTION('ref_axis',(1.,0.,0.));
#20079=DIRECTION('center_axis',(0.,1.,0.));
#20080=DIRECTION('ref_axis',(-0.309016994374948,0.,0.951056516295154));
#20081=DIRECTION('center_axis',(0.,1.,0.));
#20082=DIRECTION('ref_axis',(1.,0.,0.));
#20083=DIRECTION('center_axis',(0.,1.,0.));
#20084=DIRECTION('ref_axis',(-0.453990499739547,0.,0.891006524188368));
#20085=DIRECTION('center_axis',(0.,1.,0.));
#20086=DIRECTION('ref_axis',(1.,0.,0.));
#20087=DIRECTION('center_axis',(0.,1.,0.));
#20088=DIRECTION('ref_axis',(-0.587785252292473,0.,0.809016994374947));
#20089=DIRECTION('center_axis',(0.,1.,0.));
#20090=DIRECTION('ref_axis',(1.,0.,0.));
#20091=DIRECTION('center_axis',(0.,1.,0.));
#20092=DIRECTION('ref_axis',(-0.707106781186548,0.,0.707106781186547));
#20093=DIRECTION('center_axis',(0.,1.,0.));
#20094=DIRECTION('ref_axis',(1.,0.,0.));
#20095=DIRECTION('center_axis',(0.,1.,0.));
#20096=DIRECTION('ref_axis',(-0.809016994374947,0.,0.587785252292473));
#20097=DIRECTION('center_axis',(0.,1.,0.));
#20098=DIRECTION('ref_axis',(1.,0.,0.));
#20099=DIRECTION('center_axis',(0.,1.,0.));
#20100=DIRECTION('ref_axis',(-0.891006524188368,0.,0.453990499739547));
#20101=DIRECTION('center_axis',(0.,1.,0.));
#20102=DIRECTION('ref_axis',(1.,0.,0.));
#20103=DIRECTION('center_axis',(0.,1.,0.));
#20104=DIRECTION('ref_axis',(-0.951056516295154,0.,0.309016994374947));
#20105=DIRECTION('center_axis',(0.,1.,0.));
#20106=DIRECTION('ref_axis',(1.,0.,0.));
#20107=DIRECTION('center_axis',(0.,1.,0.));
#20108=DIRECTION('ref_axis',(-0.987688340595138,0.,0.156434465040231));
#20109=DIRECTION('center_axis',(0.,1.,0.));
#20110=DIRECTION('ref_axis',(1.,0.,0.));
#20111=DIRECTION('center_axis',(0.,1.,0.));
#20112=DIRECTION('ref_axis',(-1.,0.,-1.22464679914735E-16));
#20113=DIRECTION('center_axis',(0.,1.,0.));
#20114=DIRECTION('ref_axis',(1.,0.,0.));
#20115=DIRECTION('center_axis',(0.,1.,0.));
#20116=DIRECTION('ref_axis',(-0.987688340595138,0.,-0.156434465040231));
#20117=DIRECTION('center_axis',(0.,1.,0.));
#20118=DIRECTION('ref_axis',(1.,0.,0.));
#20119=DIRECTION('center_axis',(0.,1.,0.));
#20120=DIRECTION('ref_axis',(-0.951056516295154,0.,-0.309016994374948));
#20121=DIRECTION('center_axis',(0.,1.,0.));
#20122=DIRECTION('ref_axis',(1.,0.,0.));
#20123=DIRECTION('center_axis',(0.,1.,0.));
#20124=DIRECTION('ref_axis',(-0.891006524188368,0.,-0.453990499739547));
#20125=DIRECTION('center_axis',(0.,1.,0.));
#20126=DIRECTION('ref_axis',(1.,0.,0.));
#20127=DIRECTION('center_axis',(0.,1.,0.));
#20128=DIRECTION('ref_axis',(-0.809016994374947,0.,-0.587785252292473));
#20129=DIRECTION('center_axis',(0.,1.,0.));
#20130=DIRECTION('ref_axis',(1.,0.,0.));
#20131=DIRECTION('center_axis',(0.,1.,0.));
#20132=DIRECTION('ref_axis',(-0.707106781186547,0.,-0.707106781186548));
#20133=DIRECTION('center_axis',(0.,1.,0.));
#20134=DIRECTION('ref_axis',(1.,0.,0.));
#20135=DIRECTION('center_axis',(0.,1.,0.));
#20136=DIRECTION('ref_axis',(-0.587785252292473,0.,-0.809016994374947));
#20137=DIRECTION('center_axis',(0.,1.,0.));
#20138=DIRECTION('ref_axis',(1.,0.,0.));
#20139=DIRECTION('center_axis',(0.,1.,0.));
#20140=DIRECTION('ref_axis',(-0.453990499739547,0.,-0.891006524188368));
#20141=DIRECTION('center_axis',(0.,1.,0.));
#20142=DIRECTION('ref_axis',(1.,0.,0.));
#20143=DIRECTION('center_axis',(0.,1.,0.));
#20144=DIRECTION('ref_axis',(-0.309016994374947,0.,-0.951056516295154));
#20145=DIRECTION('center_axis',(0.,1.,0.));
#20146=DIRECTION('ref_axis',(1.,0.,0.));
#20147=DIRECTION('center_axis',(0.,1.,0.));
#20148=DIRECTION('ref_axis',(-0.156434465040231,0.,-0.987688340595138));
#20149=DIRECTION('center_axis',(0.,1.,0.));
#20150=DIRECTION('ref_axis',(1.,0.,0.));
#20151=DIRECTION('center_axis',(0.,1.,0.));
#20152=DIRECTION('ref_axis',(6.12323399573677E-17,0.,-1.));
#20153=DIRECTION('center_axis',(0.,1.,0.));
#20154=DIRECTION('ref_axis',(1.,0.,0.));
#20155=DIRECTION('center_axis',(0.,1.,0.));
#20156=DIRECTION('ref_axis',(0.156434465040231,0.,-0.987688340595138));
#20157=DIRECTION('center_axis',(0.,1.,0.));
#20158=DIRECTION('ref_axis',(1.,0.,0.));
#20159=DIRECTION('center_axis',(0.,1.,0.));
#20160=DIRECTION('ref_axis',(0.309016994374948,0.,-0.951056516295154));
#20161=DIRECTION('center_axis',(0.,1.,0.));
#20162=DIRECTION('ref_axis',(1.,0.,0.));
#20163=DIRECTION('center_axis',(0.,1.,0.));
#20164=DIRECTION('ref_axis',(0.453990499739547,0.,-0.891006524188368));
#20165=DIRECTION('center_axis',(0.,1.,0.));
#20166=DIRECTION('ref_axis',(1.,0.,0.));
#20167=DIRECTION('center_axis',(0.,1.,0.));
#20168=DIRECTION('ref_axis',(0.587785252292473,0.,-0.809016994374947));
#20169=DIRECTION('center_axis',(0.,1.,0.));
#20170=DIRECTION('ref_axis',(1.,0.,0.));
#20171=DIRECTION('center_axis',(0.,1.,0.));
#20172=DIRECTION('ref_axis',(0.707106781186548,0.,-0.707106781186547));
#20173=DIRECTION('center_axis',(0.,1.,0.));
#20174=DIRECTION('ref_axis',(1.,0.,0.));
#20175=DIRECTION('center_axis',(0.,1.,0.));
#20176=DIRECTION('ref_axis',(0.809016994374947,0.,-0.587785252292473));
#20177=DIRECTION('center_axis',(0.,1.,0.));
#20178=DIRECTION('ref_axis',(1.,0.,0.));
#20179=DIRECTION('center_axis',(0.,1.,0.));
#20180=DIRECTION('ref_axis',(0.891006524188368,0.,-0.453990499739547));
#20181=DIRECTION('center_axis',(0.,1.,0.));
#20182=DIRECTION('ref_axis',(1.,0.,0.));
#20183=DIRECTION('center_axis',(0.,1.,0.));
#20184=DIRECTION('ref_axis',(0.951056516295154,0.,-0.309016994374947));
#20185=DIRECTION('center_axis',(0.,1.,0.));
#20186=DIRECTION('ref_axis',(1.,0.,0.));
#20187=DIRECTION('center_axis',(0.,1.,0.));
#20188=DIRECTION('ref_axis',(0.987688340595138,0.,-0.156434465040231));
#20189=DIRECTION('center_axis',(0.,1.,0.));
#20190=DIRECTION('ref_axis',(1.,0.,0.));
#20191=DIRECTION('center_axis',(0.,1.,0.));
#20192=DIRECTION('ref_axis',(1.,0.,0.));
#20193=DIRECTION('center_axis',(0.,1.,0.));
#20194=DIRECTION('ref_axis',(1.,0.,0.));
#20195=DIRECTION('center_axis',(0.,-1.,0.));
#20196=DIRECTION('ref_axis',(1.,0.,0.));
#20197=DIRECTION('center_axis',(0.,-1.,0.));
#20198=DIRECTION('ref_axis',(1.,0.,0.));
#20199=DIRECTION('',(0.,1.,0.));
#20200=DIRECTION('center_axis',(0.,1.,0.));
#20201=DIRECTION('ref_axis',(1.,0.,0.));
#20202=DIRECTION('center_axis',(0.,1.,0.));
#20203=DIRECTION('ref_axis',(1.,0.,0.));
#20204=DIRECTION('center_axis',(0.,1.,0.));
#20205=DIRECTION('ref_axis',(1.,0.,0.));
#20206=DIRECTION('center_axis',(0.,-1.,0.));
#20207=DIRECTION('ref_axis',(0.987688340595138,0.,0.156434465040231));
#20208=DIRECTION('center_axis',(0.,1.,0.));
#20209=DIRECTION('ref_axis',(1.,0.,0.));
#20210=DIRECTION('center_axis',(0.,-1.,0.));
#20211=DIRECTION('ref_axis',(1.,0.,0.));
#20212=DIRECTION('center_axis',(0.,1.,0.));
#20213=DIRECTION('ref_axis',(1.,0.,0.));
#20214=DIRECTION('center_axis',(0.,-1.,0.));
#20215=DIRECTION('ref_axis',(0.987688340595138,0.,-0.156434465040231));
#20216=DIRECTION('center_axis',(0.,1.,0.));
#20217=DIRECTION('ref_axis',(1.,0.,0.));
#20218=DIRECTION('center_axis',(0.,-1.,0.));
#20219=DIRECTION('ref_axis',(0.951056516295154,0.,-0.309016994374947));
#20220=DIRECTION('center_axis',(0.,1.,0.));
#20221=DIRECTION('ref_axis',(1.,0.,0.));
#20222=DIRECTION('center_axis',(0.,-1.,0.));
#20223=DIRECTION('ref_axis',(0.891006524188368,0.,-0.453990499739547));
#20224=DIRECTION('center_axis',(0.,1.,0.));
#20225=DIRECTION('ref_axis',(1.,0.,0.));
#20226=DIRECTION('center_axis',(0.,-1.,0.));
#20227=DIRECTION('ref_axis',(0.809016994374947,0.,-0.587785252292473));
#20228=DIRECTION('center_axis',(0.,1.,0.));
#20229=DIRECTION('ref_axis',(1.,0.,0.));
#20230=DIRECTION('center_axis',(0.,-1.,0.));
#20231=DIRECTION('ref_axis',(0.707106781186548,0.,-0.707106781186547));
#20232=DIRECTION('center_axis',(0.,1.,0.));
#20233=DIRECTION('ref_axis',(1.,0.,0.));
#20234=DIRECTION('center_axis',(0.,-1.,0.));
#20235=DIRECTION('ref_axis',(0.587785252292473,0.,-0.809016994374947));
#20236=DIRECTION('center_axis',(0.,1.,0.));
#20237=DIRECTION('ref_axis',(1.,0.,0.));
#20238=DIRECTION('center_axis',(0.,-1.,0.));
#20239=DIRECTION('ref_axis',(0.453990499739547,0.,-0.891006524188368));
#20240=DIRECTION('center_axis',(0.,1.,0.));
#20241=DIRECTION('ref_axis',(1.,0.,0.));
#20242=DIRECTION('center_axis',(0.,-1.,0.));
#20243=DIRECTION('ref_axis',(0.309016994374948,0.,-0.951056516295154));
#20244=DIRECTION('center_axis',(0.,1.,0.));
#20245=DIRECTION('ref_axis',(1.,0.,0.));
#20246=DIRECTION('center_axis',(0.,-1.,0.));
#20247=DIRECTION('ref_axis',(0.156434465040231,0.,-0.987688340595138));
#20248=DIRECTION('center_axis',(0.,1.,0.));
#20249=DIRECTION('ref_axis',(1.,0.,0.));
#20250=DIRECTION('center_axis',(0.,-1.,0.));
#20251=DIRECTION('ref_axis',(6.12323399573677E-17,0.,-1.));
#20252=DIRECTION('center_axis',(0.,1.,0.));
#20253=DIRECTION('ref_axis',(1.,0.,0.));
#20254=DIRECTION('center_axis',(0.,-1.,0.));
#20255=DIRECTION('ref_axis',(-0.156434465040231,0.,-0.987688340595138));
#20256=DIRECTION('center_axis',(0.,1.,0.));
#20257=DIRECTION('ref_axis',(1.,0.,0.));
#20258=DIRECTION('center_axis',(0.,-1.,0.));
#20259=DIRECTION('ref_axis',(-0.309016994374947,0.,-0.951056516295154));
#20260=DIRECTION('center_axis',(0.,1.,0.));
#20261=DIRECTION('ref_axis',(1.,0.,0.));
#20262=DIRECTION('center_axis',(0.,-1.,0.));
#20263=DIRECTION('ref_axis',(-0.453990499739547,0.,-0.891006524188368));
#20264=DIRECTION('center_axis',(0.,1.,0.));
#20265=DIRECTION('ref_axis',(1.,0.,0.));
#20266=DIRECTION('center_axis',(0.,-1.,0.));
#20267=DIRECTION('ref_axis',(-0.587785252292473,0.,-0.809016994374947));
#20268=DIRECTION('center_axis',(0.,1.,0.));
#20269=DIRECTION('ref_axis',(1.,0.,0.));
#20270=DIRECTION('center_axis',(0.,-1.,0.));
#20271=DIRECTION('ref_axis',(-0.707106781186547,0.,-0.707106781186548));
#20272=DIRECTION('center_axis',(0.,1.,0.));
#20273=DIRECTION('ref_axis',(1.,0.,0.));
#20274=DIRECTION('center_axis',(0.,-1.,0.));
#20275=DIRECTION('ref_axis',(-0.809016994374947,0.,-0.587785252292473));
#20276=DIRECTION('center_axis',(0.,1.,0.));
#20277=DIRECTION('ref_axis',(1.,0.,0.));
#20278=DIRECTION('center_axis',(0.,-1.,0.));
#20279=DIRECTION('ref_axis',(-0.891006524188368,0.,-0.453990499739547));
#20280=DIRECTION('center_axis',(0.,1.,0.));
#20281=DIRECTION('ref_axis',(1.,0.,0.));
#20282=DIRECTION('center_axis',(0.,-1.,0.));
#20283=DIRECTION('ref_axis',(-0.951056516295154,0.,-0.309016994374948));
#20284=DIRECTION('center_axis',(0.,1.,0.));
#20285=DIRECTION('ref_axis',(1.,0.,0.));
#20286=DIRECTION('center_axis',(0.,-1.,0.));
#20287=DIRECTION('ref_axis',(-0.987688340595138,0.,-0.156434465040231));
#20288=DIRECTION('center_axis',(0.,1.,0.));
#20289=DIRECTION('ref_axis',(1.,0.,0.));
#20290=DIRECTION('center_axis',(0.,-1.,0.));
#20291=DIRECTION('ref_axis',(-1.,0.,-1.22464679914735E-16));
#20292=DIRECTION('center_axis',(0.,1.,0.));
#20293=DIRECTION('ref_axis',(1.,0.,0.));
#20294=DIRECTION('center_axis',(0.,-1.,0.));
#20295=DIRECTION('ref_axis',(-0.987688340595138,0.,0.156434465040231));
#20296=DIRECTION('center_axis',(0.,1.,0.));
#20297=DIRECTION('ref_axis',(1.,0.,0.));
#20298=DIRECTION('center_axis',(0.,-1.,0.));
#20299=DIRECTION('ref_axis',(-0.951056516295154,0.,0.309016994374947));
#20300=DIRECTION('center_axis',(0.,1.,0.));
#20301=DIRECTION('ref_axis',(1.,0.,0.));
#20302=DIRECTION('center_axis',(0.,-1.,0.));
#20303=DIRECTION('ref_axis',(-0.891006524188368,0.,0.453990499739547));
#20304=DIRECTION('center_axis',(0.,1.,0.));
#20305=DIRECTION('ref_axis',(1.,0.,0.));
#20306=DIRECTION('center_axis',(0.,-1.,0.));
#20307=DIRECTION('ref_axis',(-0.809016994374947,0.,0.587785252292473));
#20308=DIRECTION('center_axis',(0.,1.,0.));
#20309=DIRECTION('ref_axis',(1.,0.,0.));
#20310=DIRECTION('center_axis',(0.,-1.,0.));
#20311=DIRECTION('ref_axis',(-0.707106781186548,0.,0.707106781186547));
#20312=DIRECTION('center_axis',(0.,1.,0.));
#20313=DIRECTION('ref_axis',(1.,0.,0.));
#20314=DIRECTION('center_axis',(0.,-1.,0.));
#20315=DIRECTION('ref_axis',(-0.587785252292473,0.,0.809016994374947));
#20316=DIRECTION('center_axis',(0.,1.,0.));
#20317=DIRECTION('ref_axis',(1.,0.,0.));
#20318=DIRECTION('center_axis',(0.,-1.,0.));
#20319=DIRECTION('ref_axis',(-0.453990499739547,0.,0.891006524188368));
#20320=DIRECTION('center_axis',(0.,1.,0.));
#20321=DIRECTION('ref_axis',(1.,0.,0.));
#20322=DIRECTION('center_axis',(0.,-1.,0.));
#20323=DIRECTION('ref_axis',(-0.309016994374948,0.,0.951056516295154));
#20324=DIRECTION('center_axis',(0.,1.,0.));
#20325=DIRECTION('ref_axis',(1.,0.,0.));
#20326=DIRECTION('center_axis',(0.,-1.,0.));
#20327=DIRECTION('ref_axis',(-0.156434465040231,0.,0.987688340595138));
#20328=DIRECTION('center_axis',(0.,1.,0.));
#20329=DIRECTION('ref_axis',(1.,0.,0.));
#20330=DIRECTION('center_axis',(0.,-1.,0.));
#20331=DIRECTION('ref_axis',(-1.83697019872103E-16,0.,1.));
#20332=DIRECTION('center_axis',(0.,1.,0.));
#20333=DIRECTION('ref_axis',(1.,0.,0.));
#20334=DIRECTION('center_axis',(0.,-1.,0.));
#20335=DIRECTION('ref_axis',(0.156434465040231,0.,0.987688340595138));
#20336=DIRECTION('center_axis',(0.,1.,0.));
#20337=DIRECTION('ref_axis',(1.,0.,0.));
#20338=DIRECTION('center_axis',(0.,-1.,0.));
#20339=DIRECTION('ref_axis',(0.309016994374947,0.,0.951056516295154));
#20340=DIRECTION('center_axis',(0.,1.,0.));
#20341=DIRECTION('ref_axis',(1.,0.,0.));
#20342=DIRECTION('center_axis',(0.,-1.,0.));
#20343=DIRECTION('ref_axis',(0.453990499739547,0.,0.891006524188368));
#20344=DIRECTION('center_axis',(0.,1.,0.));
#20345=DIRECTION('ref_axis',(1.,0.,0.));
#20346=DIRECTION('center_axis',(0.,-1.,0.));
#20347=DIRECTION('ref_axis',(0.587785252292473,0.,0.809016994374948));
#20348=DIRECTION('center_axis',(0.,1.,0.));
#20349=DIRECTION('ref_axis',(1.,0.,0.));
#20350=DIRECTION('center_axis',(0.,-1.,0.));
#20351=DIRECTION('ref_axis',(0.707106781186547,0.,0.707106781186548));
#20352=DIRECTION('center_axis',(0.,1.,0.));
#20353=DIRECTION('ref_axis',(1.,0.,0.));
#20354=DIRECTION('center_axis',(0.,-1.,0.));
#20355=DIRECTION('ref_axis',(0.809016994374947,0.,0.587785252292473));
#20356=DIRECTION('center_axis',(0.,1.,0.));
#20357=DIRECTION('ref_axis',(1.,0.,0.));
#20358=DIRECTION('center_axis',(0.,-1.,0.));
#20359=DIRECTION('ref_axis',(0.891006524188368,0.,0.453990499739547));
#20360=DIRECTION('center_axis',(0.,1.,0.));
#20361=DIRECTION('ref_axis',(1.,0.,0.));
#20362=DIRECTION('center_axis',(0.,-1.,0.));
#20363=DIRECTION('ref_axis',(0.951056516295154,0.,0.309016994374948));
#20364=DIRECTION('center_axis',(0.,1.,0.));
#20365=DIRECTION('ref_axis',(1.,0.,0.));
#20366=DIRECTION('center_axis',(0.,1.,0.));
#20367=DIRECTION('ref_axis',(1.,0.,0.));
#20368=DIRECTION('center_axis',(0.,1.,0.));
#20369=DIRECTION('ref_axis',(1.,0.,0.));
#20370=DIRECTION('',(0.,-1.,0.));
#20371=DIRECTION('center_axis',(0.,1.,0.));
#20372=DIRECTION('ref_axis',(1.,0.,0.));
#20373=DIRECTION('center_axis',(0.,1.,0.));
#20374=DIRECTION('ref_axis',(-0.987688340595137,0.,-0.156434465040233));
#20375=DIRECTION('',(0.,-1.,0.));
#20376=DIRECTION('',(0.,1.,0.));
#20377=DIRECTION('center_axis',(0.,1.,0.));
#20378=DIRECTION('ref_axis',(1.,0.,0.));
#20379=DIRECTION('',(0.,-1.,0.));
#20380=DIRECTION('center_axis',(0.,1.,0.));
#20381=DIRECTION('ref_axis',(-0.951056516295153,0.,-0.309016994374949));
#20382=DIRECTION('',(0.,1.,0.));
#20383=DIRECTION('center_axis',(0.,1.,0.));
#20384=DIRECTION('ref_axis',(1.,0.,0.));
#20385=DIRECTION('',(0.,-1.,0.));
#20386=DIRECTION('center_axis',(0.,1.,0.));
#20387=DIRECTION('ref_axis',(-0.891006524188368,0.,-0.453990499739547));
#20388=DIRECTION('',(0.,1.,0.));
#20389=DIRECTION('center_axis',(0.,1.,0.));
#20390=DIRECTION('ref_axis',(1.,0.,0.));
#20391=DIRECTION('',(0.,-1.,0.));
#20392=DIRECTION('center_axis',(0.,1.,0.));
#20393=DIRECTION('ref_axis',(-0.809016994374948,0.,-0.587785252292473));
#20394=DIRECTION('',(0.,1.,0.));
#20395=DIRECTION('center_axis',(0.,1.,0.));
#20396=DIRECTION('ref_axis',(1.,0.,0.));
#20397=DIRECTION('',(0.,-1.,0.));
#20398=DIRECTION('center_axis',(0.,1.,0.));
#20399=DIRECTION('ref_axis',(-0.707106781186547,0.,-0.707106781186548));
#20400=DIRECTION('',(0.,1.,0.));
#20401=DIRECTION('center_axis',(0.,1.,0.));
#20402=DIRECTION('ref_axis',(1.,0.,0.));
#20403=DIRECTION('',(0.,-1.,0.));
#20404=DIRECTION('center_axis',(0.,1.,0.));
#20405=DIRECTION('ref_axis',(-0.587785252292474,0.,-0.809016994374947));
#20406=DIRECTION('',(0.,1.,0.));
#20407=DIRECTION('center_axis',(0.,1.,0.));
#20408=DIRECTION('ref_axis',(1.,0.,0.));
#20409=DIRECTION('',(0.,-1.,0.));
#20410=DIRECTION('center_axis',(0.,1.,0.));
#20411=DIRECTION('ref_axis',(-0.453990499739547,0.,-0.891006524188368));
#20412=DIRECTION('',(0.,1.,0.));
#20413=DIRECTION('center_axis',(0.,1.,0.));
#20414=DIRECTION('ref_axis',(1.,0.,0.));
#20415=DIRECTION('',(0.,-1.,0.));
#20416=DIRECTION('center_axis',(0.,1.,0.));
#20417=DIRECTION('ref_axis',(-0.309016994374948,0.,-0.951056516295153));
#20418=DIRECTION('',(0.,1.,0.));
#20419=DIRECTION('center_axis',(0.,1.,0.));
#20420=DIRECTION('ref_axis',(1.,0.,0.));
#20421=DIRECTION('',(0.,-1.,0.));
#20422=DIRECTION('center_axis',(0.,1.,0.));
#20423=DIRECTION('ref_axis',(-0.156434465040232,0.,-0.987688340595138));
#20424=DIRECTION('',(0.,1.,0.));
#20425=DIRECTION('center_axis',(0.,1.,0.));
#20426=DIRECTION('ref_axis',(1.,0.,0.));
#20427=DIRECTION('',(0.,-1.,0.));
#20428=DIRECTION('center_axis',(0.,1.,0.));
#20429=DIRECTION('ref_axis',(3.06161699786838E-16,0.,-1.));
#20430=DIRECTION('',(0.,1.,0.));
#20431=DIRECTION('center_axis',(0.,1.,0.));
#20432=DIRECTION('ref_axis',(1.,0.,0.));
#20433=DIRECTION('',(0.,-1.,0.));
#20434=DIRECTION('center_axis',(0.,1.,0.));
#20435=DIRECTION('ref_axis',(0.156434465040233,0.,-0.987688340595138));
#20436=DIRECTION('',(0.,1.,0.));
#20437=DIRECTION('center_axis',(0.,1.,0.));
#20438=DIRECTION('ref_axis',(1.,0.,0.));
#20439=DIRECTION('',(0.,-1.,0.));
#20440=DIRECTION('center_axis',(0.,1.,0.));
#20441=DIRECTION('ref_axis',(0.309016994374946,0.,-0.951056516295154));
#20442=DIRECTION('',(0.,1.,0.));
#20443=DIRECTION('center_axis',(0.,1.,0.));
#20444=DIRECTION('ref_axis',(1.,0.,0.));
#20445=DIRECTION('',(0.,-1.,0.));
#20446=DIRECTION('center_axis',(0.,1.,0.));
#20447=DIRECTION('ref_axis',(0.453990499739547,0.,-0.891006524188368));
#20448=DIRECTION('',(0.,1.,0.));
#20449=DIRECTION('center_axis',(0.,1.,0.));
#20450=DIRECTION('ref_axis',(1.,0.,0.));
#20451=DIRECTION('',(0.,-1.,0.));
#20452=DIRECTION('center_axis',(0.,1.,0.));
#20453=DIRECTION('ref_axis',(0.587785252292473,0.,-0.809016994374947));
#20454=DIRECTION('',(0.,1.,0.));
#20455=DIRECTION('center_axis',(0.,1.,0.));
#20456=DIRECTION('ref_axis',(1.,0.,0.));
#20457=DIRECTION('',(0.,-1.,0.));
#20458=DIRECTION('center_axis',(0.,1.,0.));
#20459=DIRECTION('ref_axis',(0.707106781186548,0.,-0.707106781186547));
#20460=DIRECTION('',(0.,1.,0.));
#20461=DIRECTION('center_axis',(0.,1.,0.));
#20462=DIRECTION('ref_axis',(1.,0.,0.));
#20463=DIRECTION('',(0.,-1.,0.));
#20464=DIRECTION('center_axis',(0.,1.,0.));
#20465=DIRECTION('ref_axis',(0.809016994374946,0.,-0.587785252292475));
#20466=DIRECTION('',(0.,1.,0.));
#20467=DIRECTION('center_axis',(0.,1.,0.));
#20468=DIRECTION('ref_axis',(1.,0.,0.));
#20469=DIRECTION('',(0.,-1.,0.));
#20470=DIRECTION('center_axis',(0.,1.,0.));
#20471=DIRECTION('ref_axis',(0.891006524188368,0.,-0.453990499739547));
#20472=DIRECTION('',(0.,1.,0.));
#20473=DIRECTION('center_axis',(0.,1.,0.));
#20474=DIRECTION('ref_axis',(1.,0.,0.));
#20475=DIRECTION('',(0.,-1.,0.));
#20476=DIRECTION('center_axis',(0.,1.,0.));
#20477=DIRECTION('ref_axis',(0.951056516295154,0.,-0.309016994374946));
#20478=DIRECTION('',(0.,1.,0.));
#20479=DIRECTION('center_axis',(0.,1.,0.));
#20480=DIRECTION('ref_axis',(1.,0.,0.));
#20481=DIRECTION('',(0.,-1.,0.));
#20482=DIRECTION('center_axis',(0.,1.,0.));
#20483=DIRECTION('ref_axis',(0.987688340595138,0.,-0.156434465040232));
#20484=DIRECTION('',(0.,1.,0.));
#20485=DIRECTION('center_axis',(0.,1.,0.));
#20486=DIRECTION('ref_axis',(1.,0.,0.));
#20487=DIRECTION('',(0.,-1.,0.));
#20488=DIRECTION('center_axis',(0.,1.,0.));
#20489=DIRECTION('ref_axis',(1.,0.,2.44929359829471E-16));
#20490=DIRECTION('',(0.,1.,0.));
#20491=DIRECTION('center_axis',(0.,1.,0.));
#20492=DIRECTION('ref_axis',(1.,0.,0.));
#20493=DIRECTION('',(0.,-1.,0.));
#20494=DIRECTION('center_axis',(0.,1.,0.));
#20495=DIRECTION('ref_axis',(0.987688340595137,0.,0.156434465040232));
#20496=DIRECTION('',(0.,1.,0.));
#20497=DIRECTION('center_axis',(0.,1.,0.));
#20498=DIRECTION('ref_axis',(1.,0.,0.));
#20499=DIRECTION('',(0.,-1.,0.));
#20500=DIRECTION('center_axis',(0.,1.,0.));
#20501=DIRECTION('ref_axis',(0.951056516295154,0.,0.309016994374946));
#20502=DIRECTION('',(0.,1.,0.));
#20503=DIRECTION('center_axis',(0.,1.,0.));
#20504=DIRECTION('ref_axis',(1.,0.,0.));
#20505=DIRECTION('',(0.,-1.,0.));
#20506=DIRECTION('center_axis',(0.,1.,0.));
#20507=DIRECTION('ref_axis',(0.891006524188368,0.,0.453990499739547));
#20508=DIRECTION('',(0.,1.,0.));
#20509=DIRECTION('center_axis',(0.,1.,0.));
#20510=DIRECTION('ref_axis',(1.,0.,0.));
#20511=DIRECTION('',(0.,-1.,0.));
#20512=DIRECTION('center_axis',(0.,1.,0.));
#20513=DIRECTION('ref_axis',(0.809016994374947,0.,0.587785252292473));
#20514=DIRECTION('',(0.,1.,0.));
#20515=DIRECTION('center_axis',(0.,1.,0.));
#20516=DIRECTION('ref_axis',(1.,0.,0.));
#20517=DIRECTION('',(0.,-1.,0.));
#20518=DIRECTION('center_axis',(0.,1.,0.));
#20519=DIRECTION('ref_axis',(0.707106781186547,0.,0.707106781186548));
#20520=DIRECTION('',(0.,1.,0.));
#20521=DIRECTION('center_axis',(0.,1.,0.));
#20522=DIRECTION('ref_axis',(1.,0.,0.));
#20523=DIRECTION('',(0.,-1.,0.));
#20524=DIRECTION('center_axis',(0.,1.,0.));
#20525=DIRECTION('ref_axis',(0.587785252292475,0.,0.809016994374946));
#20526=DIRECTION('',(0.,1.,0.));
#20527=DIRECTION('center_axis',(0.,1.,0.));
#20528=DIRECTION('ref_axis',(1.,0.,0.));
#20529=DIRECTION('',(0.,-1.,0.));
#20530=DIRECTION('center_axis',(0.,1.,0.));
#20531=DIRECTION('ref_axis',(0.453990499739547,0.,0.891006524188368));
#20532=DIRECTION('',(0.,1.,0.));
#20533=DIRECTION('center_axis',(0.,1.,0.));
#20534=DIRECTION('ref_axis',(1.,0.,0.));
#20535=DIRECTION('',(0.,-1.,0.));
#20536=DIRECTION('center_axis',(0.,1.,0.));
#20537=DIRECTION('ref_axis',(0.309016994374946,0.,0.951056516295154));
#20538=DIRECTION('',(0.,1.,0.));
#20539=DIRECTION('center_axis',(0.,1.,0.));
#20540=DIRECTION('ref_axis',(1.,0.,0.));
#20541=DIRECTION('',(0.,-1.,0.));
#20542=DIRECTION('center_axis',(0.,1.,0.));
#20543=DIRECTION('ref_axis',(0.156434465040232,0.,0.987688340595138));
#20544=DIRECTION('',(0.,1.,0.));
#20545=DIRECTION('center_axis',(0.,1.,0.));
#20546=DIRECTION('ref_axis',(1.,0.,0.));
#20547=DIRECTION('',(0.,-1.,0.));
#20548=DIRECTION('center_axis',(0.,1.,0.));
#20549=DIRECTION('ref_axis',(-1.83697019872103E-16,0.,1.));
#20550=DIRECTION('',(0.,1.,0.));
#20551=DIRECTION('center_axis',(0.,1.,0.));
#20552=DIRECTION('ref_axis',(1.,0.,0.));
#20553=DIRECTION('',(0.,-1.,0.));
#20554=DIRECTION('center_axis',(0.,1.,0.));
#20555=DIRECTION('ref_axis',(-0.156434465040232,0.,0.987688340595138));
#20556=DIRECTION('',(0.,1.,0.));
#20557=DIRECTION('center_axis',(0.,1.,0.));
#20558=DIRECTION('ref_axis',(1.,0.,0.));
#20559=DIRECTION('',(0.,-1.,0.));
#20560=DIRECTION('center_axis',(0.,1.,0.));
#20561=DIRECTION('ref_axis',(-0.309016994374946,0.,0.951056516295154));
#20562=DIRECTION('',(0.,1.,0.));
#20563=DIRECTION('center_axis',(0.,1.,0.));
#20564=DIRECTION('ref_axis',(1.,0.,0.));
#20565=DIRECTION('',(0.,-1.,0.));
#20566=DIRECTION('center_axis',(0.,1.,0.));
#20567=DIRECTION('ref_axis',(-0.453990499739549,0.,0.891006524188367));
#20568=DIRECTION('',(0.,1.,0.));
#20569=DIRECTION('center_axis',(0.,1.,0.));
#20570=DIRECTION('ref_axis',(1.,0.,0.));
#20571=DIRECTION('',(0.,-1.,0.));
#20572=DIRECTION('center_axis',(0.,1.,0.));
#20573=DIRECTION('ref_axis',(-0.587785252292474,0.,0.809016994374947));
#20574=DIRECTION('',(0.,1.,0.));
#20575=DIRECTION('center_axis',(0.,1.,0.));
#20576=DIRECTION('ref_axis',(1.,0.,0.));
#20577=DIRECTION('',(0.,-1.,0.));
#20578=DIRECTION('center_axis',(0.,1.,0.));
#20579=DIRECTION('ref_axis',(-0.707106781186548,0.,0.707106781186547));
#20580=DIRECTION('',(0.,1.,0.));
#20581=DIRECTION('center_axis',(0.,1.,0.));
#20582=DIRECTION('ref_axis',(1.,0.,0.));
#20583=DIRECTION('',(0.,-1.,0.));
#20584=DIRECTION('center_axis',(0.,1.,0.));
#20585=DIRECTION('ref_axis',(-0.809016994374947,0.,0.587785252292474));
#20586=DIRECTION('',(0.,1.,0.));
#20587=DIRECTION('center_axis',(0.,1.,0.));
#20588=DIRECTION('ref_axis',(1.,0.,0.));
#20589=DIRECTION('',(0.,-1.,0.));
#20590=DIRECTION('center_axis',(0.,1.,0.));
#20591=DIRECTION('ref_axis',(-0.891006524188368,0.,0.453990499739547));
#20592=DIRECTION('',(0.,1.,0.));
#20593=DIRECTION('center_axis',(0.,1.,0.));
#20594=DIRECTION('ref_axis',(1.,0.,0.));
#20595=DIRECTION('',(0.,-1.,0.));
#20596=DIRECTION('center_axis',(0.,1.,0.));
#20597=DIRECTION('ref_axis',(-0.951056516295154,0.,0.309016994374948));
#20598=DIRECTION('',(0.,1.,0.));
#20599=DIRECTION('center_axis',(0.,1.,0.));
#20600=DIRECTION('ref_axis',(1.,0.,0.));
#20601=DIRECTION('',(0.,-1.,0.));
#20602=DIRECTION('center_axis',(0.,1.,0.));
#20603=DIRECTION('ref_axis',(-0.987688340595137,0.,0.156434465040233));
#20604=DIRECTION('',(0.,1.,0.));
#20605=DIRECTION('center_axis',(0.,1.,0.));
#20606=DIRECTION('ref_axis',(1.,0.,0.));
#20607=DIRECTION('',(0.,1.,0.));
#20608=DIRECTION('center_axis',(0.,1.,0.));
#20609=DIRECTION('ref_axis',(-1.,0.,-1.22464679914735E-16));
#20610=DIRECTION('',(0.,-1.,0.));
#20611=DIRECTION('center_axis',(0.,1.,0.));
#20612=DIRECTION('ref_axis',(1.,0.,0.));
#20613=DIRECTION('axis',(0.,0.,1.));
#20614=DIRECTION('refdir',(1.,0.,0.));
#20615=DIRECTION('center_axis',(0.,1.,0.));
#20616=DIRECTION('ref_axis',(0.,0.,1.));
#20617=DIRECTION('center_axis',(0.,-1.,0.));
#20618=DIRECTION('ref_axis',(1.,0.,0.));
#20619=DIRECTION('center_axis',(0.,-1.,0.));
#20620=DIRECTION('ref_axis',(1.,0.,0.));
#20621=DIRECTION('center_axis',(0.,-1.,0.));
#20622=DIRECTION('ref_axis',(1.,0.,0.));
#20623=DIRECTION('',(0.707106781186547,0.707106781186548,8.65956056235493E-17));
#20624=DIRECTION('center_axis',(0.,-1.,0.));
#20625=DIRECTION('ref_axis',(1.,0.,0.));
#20626=DIRECTION('center_axis',(0.,-1.,0.));
#20627=DIRECTION('ref_axis',(1.,0.,0.));
#20628=DIRECTION('',(0.,1.,0.));
#20629=DIRECTION('center_axis',(0.,1.,0.));
#20630=DIRECTION('ref_axis',(1.,0.,0.));
#20631=DIRECTION('center_axis',(0.,-1.,0.));
#20632=DIRECTION('ref_axis',(1.,0.,0.));
#20633=DIRECTION('',(-0.707106781186547,0.707106781186548,-8.65956056235493E-17));
#20634=DIRECTION('center_axis',(0.,-1.,0.));
#20635=DIRECTION('ref_axis',(0.,0.,-1.));
#20636=DIRECTION('center_axis',(0.,-1.,0.));
#20637=DIRECTION('ref_axis',(1.,0.,0.));
#20638=DIRECTION('center_axis',(0.,1.,0.));
#20639=DIRECTION('ref_axis',(1.,0.,0.));
#20640=DIRECTION('center_axis',(0.,1.,0.));
#20641=DIRECTION('ref_axis',(1.,0.,0.));
#20642=DIRECTION('',(-0.447213595499958,0.894427190999916,-5.47678698264203E-17));
#20643=DIRECTION('center_axis',(0.,-1.,0.));
#20644=DIRECTION('ref_axis',(1.,0.,0.));
#20645=DIRECTION('center_axis',(0.,1.,0.));
#20646=DIRECTION('ref_axis',(1.,0.,0.));
#20647=DIRECTION('',(0.,1.,0.));
#20648=DIRECTION('center_axis',(0.,1.,0.));
#20649=DIRECTION('ref_axis',(1.,0.,0.));
#20650=DIRECTION('center_axis',(0.,-1.,0.));
#20651=DIRECTION('ref_axis',(1.,0.,0.));
#20652=DIRECTION('',(-0.707106781186547,0.707106781186548,-8.65956056235493E-17));
#20653=DIRECTION('center_axis',(0.,-1.,0.));
#20654=DIRECTION('ref_axis',(0.,0.,-1.));
#20655=DIRECTION('center_axis',(0.866025403784439,0.,-0.5));
#20656=DIRECTION('ref_axis',(0.5,0.,0.866025403784439));
#20657=DIRECTION('',(-0.5,0.,-0.866025403784439));
#20658=DIRECTION('',(0.,-1.,0.));
#20659=DIRECTION('',(0.5,0.,0.866025403784439));
#20660=DIRECTION('',(0.,-1.,0.));
#20661=DIRECTION('center_axis',(1.60246890531964E-16,0.,-1.));
#20662=DIRECTION('ref_axis',(1.,0.,1.60246890531964E-16));
#20663=DIRECTION('',(-1.,0.,-1.60246890531964E-16));
#20664=DIRECTION('',(0.,-1.,0.));
#20665=DIRECTION('',(1.,0.,1.60246890531964E-16));
#20666=DIRECTION('center_axis',(-0.866025403784439,0.,-0.5));
#20667=DIRECTION('ref_axis',(0.5,0.,-0.866025403784439));
#20668=DIRECTION('',(-0.5,0.,0.866025403784439));
#20669=DIRECTION('',(0.,-1.,0.));
#20670=DIRECTION('',(0.5,0.,-0.866025403784439));
#20671=DIRECTION('center_axis',(-0.866025403784439,0.,0.5));
#20672=DIRECTION('ref_axis',(-0.5,0.,-0.866025403784439));
#20673=DIRECTION('',(0.5,0.,0.866025403784439));
#20674=DIRECTION('',(0.,-1.,0.));
#20675=DIRECTION('',(-0.5,0.,-0.866025403784439));
#20676=DIRECTION('center_axis',(-1.60246890531964E-16,0.,1.));
#20677=DIRECTION('ref_axis',(-1.,0.,-1.60246890531964E-16));
#20678=DIRECTION('',(1.,0.,1.60246890531964E-16));
#20679=DIRECTION('',(0.,-1.,0.));
#20680=DIRECTION('',(-1.,0.,-1.60246890531964E-16));
#20681=DIRECTION('center_axis',(0.866025403784439,0.,0.5));
#20682=DIRECTION('ref_axis',(-0.5,0.,0.866025403784439));
#20683=DIRECTION('',(0.5,0.,-0.866025403784439));
#20684=DIRECTION('',(-0.5,0.,0.866025403784439));
#20685=DIRECTION('center_axis',(0.,1.,0.));
#20686=DIRECTION('ref_axis',(1.,0.,0.));
#20687=DIRECTION('center_axis',(0.,-1.,0.));
#20688=DIRECTION('ref_axis',(0.,0.,-1.));
#20689=DIRECTION('',(0.,0.,1.));
#20690=DIRECTION('',(1.,0.,0.));
#20691=DIRECTION('',(0.,0.,1.));
#20692=DIRECTION('',(1.,0.,0.));
#20693=DIRECTION('',(0.,0.,1.));
#20694=DIRECTION('',(1.,0.,0.));
#20695=DIRECTION('',(0.,0.,1.));
#20696=DIRECTION('',(1.,0.,0.));
#20697=DIRECTION('',(0.,0.,1.));
#20698=DIRECTION('',(1.,0.,0.));
#20699=DIRECTION('',(0.,0.,1.));
#20700=DIRECTION('',(1.,0.,0.));
#20701=DIRECTION('',(0.,0.,1.));
#20702=DIRECTION('',(1.,0.,0.));
#20703=DIRECTION('',(0.,0.,1.));
#20704=DIRECTION('',(1.,0.,0.));
#20705=DIRECTION('',(0.,0.,1.));
#20706=DIRECTION('',(1.,0.,0.));
#20707=DIRECTION('',(0.,0.,1.));
#20708=DIRECTION('',(1.,0.,0.));
#20709=DIRECTION('',(0.,0.,1.));
#20710=DIRECTION('',(1.,0.,0.));
#20711=DIRECTION('',(0.,0.,1.));
#20712=DIRECTION('',(1.,0.,0.));
#20713=DIRECTION('',(0.,0.,1.));
#20714=DIRECTION('',(1.,0.,0.));
#20715=DIRECTION('',(0.,0.,1.));
#20716=DIRECTION('',(1.,0.,0.));
#20717=DIRECTION('',(0.,0.,1.));
#20718=DIRECTION('',(1.,0.,0.));
#20719=DIRECTION('',(0.,0.,1.));
#20720=DIRECTION('',(1.,0.,0.));
#20721=DIRECTION('',(0.,0.,1.));
#20722=DIRECTION('',(1.,0.,0.));
#20723=DIRECTION('',(0.,0.,1.));
#20724=DIRECTION('',(1.,0.,0.));
#20725=DIRECTION('',(0.,0.,1.));
#20726=DIRECTION('',(1.,0.,0.));
#20727=DIRECTION('',(0.,0.,1.));
#20728=DIRECTION('',(1.,0.,0.));
#20729=DIRECTION('',(0.,0.,1.));
#20730=DIRECTION('',(1.,0.,0.));
#20731=DIRECTION('',(0.,0.,1.));
#20732=DIRECTION('',(1.,0.,0.));
#20733=DIRECTION('',(0.,0.,1.));
#20734=DIRECTION('',(1.,0.,0.));
#20735=DIRECTION('',(0.,0.,1.));
#20736=DIRECTION('',(1.,0.,0.));
#20737=DIRECTION('',(0.,0.,1.));
#20738=DIRECTION('',(1.,0.,0.));
#20739=DIRECTION('',(0.,0.,1.));
#20740=DIRECTION('',(1.,0.,0.));
#20741=DIRECTION('',(0.,0.,1.));
#20742=DIRECTION('',(1.,0.,0.));
#20743=DIRECTION('',(0.,-1.,2.22044604925031E-16));
#20744=DIRECTION('',(1.,0.,0.));
#20745=DIRECTION('',(0.,-1.,2.22044604925031E-16));
#20746=DIRECTION('',(1.,0.,0.));
#20747=DIRECTION('',(0.,-1.,2.22044604925031E-16));
#20748=DIRECTION('',(1.,0.,0.));
#20749=DIRECTION('',(0.,-1.,2.22044604925031E-16));
#20750=DIRECTION('',(1.,0.,0.));
#20751=DIRECTION('',(0.,0.,1.));
#20752=DIRECTION('',(1.,0.,0.));
#20753=DIRECTION('',(0.,0.,1.));
#20754=DIRECTION('',(1.,0.,0.));
#20755=DIRECTION('',(0.,0.,1.));
#20756=DIRECTION('',(-1.,1.22464679914735E-16,0.));
#20757=DIRECTION('',(0.,0.,1.));
#20758=DIRECTION('',(-1.,1.22464679914735E-16,0.));
#20759=DIRECTION('',(0.,0.,1.));
#20760=DIRECTION('',(-1.,1.22464679914735E-16,0.));
#20761=DIRECTION('',(0.,0.,1.));
#20762=DIRECTION('',(-1.,1.22464679914735E-16,0.));
#20763=DIRECTION('',(0.,0.,1.));
#20764=DIRECTION('',(1.,0.,0.));
#20765=DIRECTION('',(0.,0.,1.));
#20766=DIRECTION('',(1.,0.,0.));
#20767=DIRECTION('',(0.,0.,1.));
#20768=DIRECTION('',(1.,0.,0.));
#20769=DIRECTION('',(0.,0.,1.));
#20770=DIRECTION('',(1.,0.,0.));
#20771=DIRECTION('',(0.,-1.,2.22044604925031E-16));
#20772=DIRECTION('',(1.,0.,0.));
#20773=DIRECTION('',(0.,-1.,2.22044604925031E-16));
#20774=DIRECTION('',(1.,0.,0.));
#20775=DIRECTION('',(0.,-1.,2.22044604925031E-16));
#20776=DIRECTION('',(1.,0.,0.));
#20777=DIRECTION('',(0.,-1.,2.22044604925031E-16));
#20778=DIRECTION('',(1.,0.,0.));
#20779=DIRECTION('',(0.,0.,1.));
#20780=DIRECTION('',(1.,0.,0.));
#20781=DIRECTION('',(0.,0.,1.));
#20782=DIRECTION('',(1.,0.,0.));
#20783=DIRECTION('',(0.,0.,1.));
#20784=DIRECTION('',(-1.,1.22464679914735E-16,0.));
#20785=DIRECTION('',(0.,0.,1.));
#20786=DIRECTION('',(-1.,1.22464679914735E-16,0.));
#20787=DIRECTION('',(0.,0.,1.));
#20788=DIRECTION('',(-1.,1.22464679914735E-16,0.));
#20789=DIRECTION('',(0.,0.,1.));
#20790=DIRECTION('',(-1.,1.22464679914735E-16,0.));
#20791=DIRECTION('',(0.,0.,1.));
#20792=DIRECTION('',(1.,0.,0.));
#20793=DIRECTION('',(0.,0.,1.));
#20794=DIRECTION('',(1.,0.,0.));
#20795=DIRECTION('',(0.,0.,1.));
#20796=DIRECTION('',(1.,0.,0.));
#20797=DIRECTION('',(0.,0.,1.));
#20798=DIRECTION('',(1.,0.,0.));
#20799=DIRECTION('',(0.,-1.,2.22044604925031E-16));
#20800=DIRECTION('',(1.,0.,0.));
#20801=DIRECTION('',(0.,-1.,2.22044604925031E-16));
#20802=DIRECTION('',(1.,0.,0.));
#20803=DIRECTION('',(0.,-1.,2.22044604925031E-16));
#20804=DIRECTION('',(1.,0.,0.));
#20805=DIRECTION('',(0.,-1.,2.22044604925031E-16));
#20806=DIRECTION('',(1.,0.,0.));
#20807=DIRECTION('',(0.,0.,1.));
#20808=DIRECTION('',(1.,0.,0.));
#20809=DIRECTION('',(0.,-1.,2.22044604925031E-16));
#20810=DIRECTION('',(1.,0.,0.));
#20811=DIRECTION('',(0.,-1.,2.22044604925031E-16));
#20812=DIRECTION('',(1.,0.,0.));
#20813=DIRECTION('',(0.,-1.,2.22044604925031E-16));
#20814=DIRECTION('',(1.,0.,0.));
#20815=DIRECTION('',(0.,-1.,2.22044604925031E-16));
#20816=DIRECTION('',(1.,0.,0.));
#20817=DIRECTION('',(0.,-1.,2.22044604925031E-16));
#20818=DIRECTION('',(1.,0.,0.));
#20819=DIRECTION('',(0.,-1.,2.22044604925031E-16));
#20820=DIRECTION('',(1.,0.,0.));
#20821=DIRECTION('',(0.,-1.,2.22044604925031E-16));
#20822=DIRECTION('',(1.,0.,0.));
#20823=DIRECTION('',(0.,-1.,2.22044604925031E-16));
#20824=DIRECTION('',(1.,0.,0.));
#20825=DIRECTION('',(0.,0.,1.));
#20826=DIRECTION('',(1.,0.,0.));
#20827=DIRECTION('',(0.,-1.,2.22044604925031E-16));
#20828=DIRECTION('',(1.,0.,0.));
#20829=DIRECTION('',(0.,-1.,2.22044604925031E-16));
#20830=DIRECTION('',(1.,0.,0.));
#20831=DIRECTION('',(0.,-1.,2.22044604925031E-16));
#20832=DIRECTION('',(1.,0.,0.));
#20833=DIRECTION('',(0.,-1.,2.22044604925031E-16));
#20834=DIRECTION('',(1.,0.,0.));
#20835=DIRECTION('',(0.,-1.,2.22044604925031E-16));
#20836=DIRECTION('',(1.,0.,0.));
#20837=DIRECTION('',(0.,-1.,2.22044604925031E-16));
#20838=DIRECTION('',(1.,0.,0.));
#20839=DIRECTION('',(0.,0.,1.));
#20840=DIRECTION('',(-1.,1.22464679914735E-16,0.));
#20841=DIRECTION('',(0.,0.,1.));
#20842=DIRECTION('',(-1.,1.22464679914735E-16,0.));
#20843=DIRECTION('',(0.,0.,1.));
#20844=DIRECTION('',(-1.,1.22464679914735E-16,0.));
#20845=DIRECTION('',(0.,0.,1.));
#20846=DIRECTION('',(-1.,1.22464679914735E-16,0.));
#20847=DIRECTION('axis',(0.,0.,1.));
#20848=DIRECTION('refdir',(1.,0.,0.));
#20849=DIRECTION('center_axis',(0.866025403784439,0.,-0.5));
#20850=DIRECTION('ref_axis',(0.5,0.,0.866025403784439));
#20851=DIRECTION('',(0.5,0.,0.866025403784439));
#20852=DIRECTION('',(0.,-1.,0.));
#20853=DIRECTION('',(0.5,0.,0.866025403784439));
#20854=DIRECTION('',(0.,-1.,0.));
#20855=DIRECTION('center_axis',(1.92296268638356E-16,0.,-1.));
#20856=DIRECTION('ref_axis',(1.,0.,1.92296268638356E-16));
#20857=DIRECTION('',(1.,0.,1.92296268638356E-16));
#20858=DIRECTION('',(0.,-1.,0.));
#20859=DIRECTION('',(1.,0.,1.92296268638356E-16));
#20860=DIRECTION('center_axis',(-0.866025403784439,0.,-0.5));
#20861=DIRECTION('ref_axis',(0.5,0.,-0.866025403784439));
#20862=DIRECTION('',(0.5,0.,-0.866025403784439));
#20863=DIRECTION('',(0.,-1.,0.));
#20864=DIRECTION('',(0.5,0.,-0.866025403784438));
#20865=DIRECTION('center_axis',(-0.866025403784439,0.,0.5));
#20866=DIRECTION('ref_axis',(-0.5,0.,-0.866025403784439));
#20867=DIRECTION('',(-0.5,0.,-0.866025403784439));
#20868=DIRECTION('',(0.,-1.,0.));
#20869=DIRECTION('',(-0.5,0.,-0.866025403784439));
#20870=DIRECTION('center_axis',(-1.92296268638356E-16,0.,1.));
#20871=DIRECTION('ref_axis',(-1.,0.,-1.92296268638356E-16));
#20872=DIRECTION('',(-1.,0.,-1.92296268638356E-16));
#20873=DIRECTION('',(0.,-1.,0.));
#20874=DIRECTION('',(-1.,0.,-1.92296268638356E-16));
#20875=DIRECTION('center_axis',(0.866025403784439,0.,0.5));
#20876=DIRECTION('ref_axis',(-0.5,0.,0.866025403784439));
#20877=DIRECTION('',(-0.5,0.,0.866025403784439));
#20878=DIRECTION('',(-0.5,0.,0.866025403784439));
#20879=DIRECTION('center_axis',(0.,-1.,0.));
#20880=DIRECTION('ref_axis',(0.,0.,-1.));
#20881=DIRECTION('center_axis',(0.,1.,0.));
#20882=DIRECTION('ref_axis',(0.,0.,1.));
#20883=DIRECTION('center_axis',(0.,-1.,0.));
#20884=DIRECTION('ref_axis',(1.,0.,0.));
#20885=DIRECTION('center_axis',(0.,-1.,0.));
#20886=DIRECTION('ref_axis',(1.,0.,0.));
#20887=DIRECTION('center_axis',(0.,-1.,0.));
#20888=DIRECTION('ref_axis',(1.,0.,0.));
#20889=DIRECTION('',(0.707106781186547,0.707106781186548,8.65956056235493E-17));
#20890=DIRECTION('center_axis',(0.,-1.,0.));
#20891=DIRECTION('ref_axis',(1.,0.,0.));
#20892=DIRECTION('center_axis',(0.,1.,0.));
#20893=DIRECTION('ref_axis',(1.,0.,0.));
#20894=DIRECTION('',(0.,1.,0.));
#20895=DIRECTION('center_axis',(0.,1.,0.));
#20896=DIRECTION('ref_axis',(1.,0.,0.));
#20897=DIRECTION('center_axis',(0.,-1.,0.));
#20898=DIRECTION('ref_axis',(1.,0.,0.));
#20899=DIRECTION('',(-0.707106781186547,0.707106781186548,-8.65956056235493E-17));
#20900=DIRECTION('center_axis',(0.,-1.,0.));
#20901=DIRECTION('ref_axis',(0.,0.,-1.));
#20902=DIRECTION('',(0.,0.,1.));
#20903=DIRECTION('',(1.,0.,0.));
#20904=DIRECTION('',(0.,0.,1.));
#20905=DIRECTION('',(1.,0.,0.));
#20906=DIRECTION('',(0.,0.,1.));
#20907=DIRECTION('',(1.,0.,0.));
#20908=DIRECTION('',(0.,0.,1.));
#20909=DIRECTION('',(1.,0.,0.));
#20910=DIRECTION('',(0.,0.,1.));
#20911=DIRECTION('',(1.,0.,0.));
#20912=DIRECTION('',(0.,0.,1.));
#20913=DIRECTION('',(1.,0.,0.));
#20914=DIRECTION('',(0.,0.,1.));
#20915=DIRECTION('',(1.,0.,0.));
#20916=DIRECTION('',(0.,0.,1.));
#20917=DIRECTION('',(1.,0.,0.));
#20918=DIRECTION('',(0.,0.,1.));
#20919=DIRECTION('',(1.,0.,0.));
#20920=DIRECTION('',(0.,0.,1.));
#20921=DIRECTION('',(-1.,1.22464679914735E-16,0.));
#20922=DIRECTION('',(0.,-1.,2.22044604925031E-16));
#20923=DIRECTION('',(1.,0.,0.));
#20924=DIRECTION('',(0.,-1.,2.22044604925031E-16));
#20925=DIRECTION('',(1.,0.,0.));
#20926=DIRECTION('',(0.,0.,1.));
#20927=DIRECTION('',(1.,0.,0.));
#20928=DIRECTION('',(0.,0.,1.));
#20929=DIRECTION('',(1.,0.,0.));
#20930=DIRECTION('',(0.,0.,1.));
#20931=DIRECTION('',(1.,0.,0.));
#20932=DIRECTION('',(0.,0.,1.));
#20933=DIRECTION('',(1.,0.,0.));
#20934=DIRECTION('',(0.,0.,1.));
#20935=DIRECTION('',(1.,0.,0.));
#20936=DIRECTION('',(0.,0.,1.));
#20937=DIRECTION('',(1.,0.,0.));
#20938=DIRECTION('',(0.,0.,1.));
#20939=DIRECTION('',(1.,0.,0.));
#20940=DIRECTION('',(0.,0.,1.));
#20941=DIRECTION('',(1.,0.,0.));
#20942=DIRECTION('',(0.,0.,1.));
#20943=DIRECTION('',(1.,0.,0.));
#20944=DIRECTION('',(0.,0.,1.));
#20945=DIRECTION('',(1.,0.,0.));
#20946=DIRECTION('',(0.,0.,1.));
#20947=DIRECTION('',(1.,0.,0.));
#20948=DIRECTION('',(0.,0.,1.));
#20949=DIRECTION('',(1.,0.,0.));
#20950=DIRECTION('',(0.,0.,1.));
#20951=DIRECTION('',(1.,0.,0.));
#20952=DIRECTION('',(0.,0.,1.));
#20953=DIRECTION('',(1.,0.,0.));
#20954=DIRECTION('',(0.,0.,1.));
#20955=DIRECTION('',(-1.,1.22464679914735E-16,0.));
#20956=DIRECTION('',(0.,-1.,2.22044604925031E-16));
#20957=DIRECTION('',(1.,0.,0.));
#20958=DIRECTION('',(0.,-1.,2.22044604925031E-16));
#20959=DIRECTION('',(1.,0.,0.));
#20960=DIRECTION('',(0.,-1.,2.22044604925031E-16));
#20961=DIRECTION('',(1.,0.,0.));
#20962=DIRECTION('',(0.,-1.,2.22044604925031E-16));
#20963=DIRECTION('',(1.,0.,0.));
#20964=DIRECTION('',(0.,0.,1.));
#20965=DIRECTION('',(1.,0.,0.));
#20966=DIRECTION('',(0.,0.,1.));
#20967=DIRECTION('',(1.,0.,0.));
#20968=DIRECTION('',(0.,0.,1.));
#20969=DIRECTION('',(1.,0.,0.));
#20970=CARTESIAN_POINT('',(0.,0.,0.));
#20971=CARTESIAN_POINT('',(0.,0.,0.));
#20972=CARTESIAN_POINT('',(0.,0.,0.));
#20973=CARTESIAN_POINT('Origin',(-1.5,8.5,-0.9));
#20974=CARTESIAN_POINT('',(-1.665,8.5,-0.9));
#20975=CARTESIAN_POINT('Origin',(-1.5,8.5,-0.9));
#20976=CARTESIAN_POINT('',(-1.665,8.5,0.));
#20977=CARTESIAN_POINT('',(-1.665,8.5,-0.9));
#20978=CARTESIAN_POINT('Origin',(-1.5,8.5,0.));
#20979=CARTESIAN_POINT('Origin',(-1.5,8.5,-0.9));
#20980=CARTESIAN_POINT('Origin',(-1.5,4.5,-0.9));
#20981=CARTESIAN_POINT('',(-1.665,4.5,-0.9));
#20982=CARTESIAN_POINT('Origin',(-1.5,4.5,-0.9));
#20983=CARTESIAN_POINT('',(-1.665,4.5,0.));
#20984=CARTESIAN_POINT('',(-1.665,4.5,-0.9));
#20985=CARTESIAN_POINT('Origin',(-1.5,4.5,0.));
#20986=CARTESIAN_POINT('Origin',(-1.5,4.5,-0.9));
#20987=CARTESIAN_POINT('Origin',(12.7709100301812,41.5,-1.1));
#20988=CARTESIAN_POINT('',(12.5609100301812,41.5,-1.1));
#20989=CARTESIAN_POINT('Origin',(12.7709100301812,41.5,-1.1));
#20990=CARTESIAN_POINT('',(12.5609100301812,41.5,0.));
#20991=CARTESIAN_POINT('',(12.5609100301812,41.5,-1.1));
#20992=CARTESIAN_POINT('Origin',(12.7709100301812,41.5,0.));
#20993=CARTESIAN_POINT('Origin',(12.7709100301812,41.5,-1.1));
#20994=CARTESIAN_POINT('Origin',(12.7709100301812,38.5,-1.1));
#20995=CARTESIAN_POINT('',(12.5609100301812,38.5,-1.1));
#20996=CARTESIAN_POINT('Origin',(12.7709100301812,38.5,-1.1));
#20997=CARTESIAN_POINT('',(12.5609100301812,38.5,0.));
#20998=CARTESIAN_POINT('',(12.5609100301812,38.5,-1.1));
#20999=CARTESIAN_POINT('Origin',(12.7709100301812,38.5,0.));
#21000=CARTESIAN_POINT('Origin',(12.7709100301812,38.5,-1.1));
#21001=CARTESIAN_POINT('Origin',(1.17091003018116,41.5,-1.1));
#21002=CARTESIAN_POINT('',(0.960910030181156,41.5,-1.1));
#21003=CARTESIAN_POINT('Origin',(1.17091003018116,41.5,-1.1));
#21004=CARTESIAN_POINT('',(0.960910030181156,41.5,0.));
#21005=CARTESIAN_POINT('',(0.960910030181156,41.5,-1.1));
#21006=CARTESIAN_POINT('Origin',(1.17091003018116,41.5,0.));
#21007=CARTESIAN_POINT('Origin',(1.17091003018116,41.5,-1.1));
#21008=CARTESIAN_POINT('Origin',(1.17091003018116,38.5,-1.1));
#21009=CARTESIAN_POINT('',(0.960910030181156,38.5,-1.1));
#21010=CARTESIAN_POINT('Origin',(1.17091003018116,38.5,-1.1));
#21011=CARTESIAN_POINT('',(0.960910030181156,38.5,0.));
#21012=CARTESIAN_POINT('',(0.960910030181156,38.5,-1.1));
#21013=CARTESIAN_POINT('Origin',(1.17091003018116,38.5,0.));
#21014=CARTESIAN_POINT('Origin',(1.17091003018116,38.5,-1.1));
#21015=CARTESIAN_POINT('Origin',(12.7709100301812,5.5,-1.1));
#21016=CARTESIAN_POINT('',(12.5609100301812,5.5,-1.1));
#21017=CARTESIAN_POINT('Origin',(12.7709100301812,5.5,-1.1));
#21018=CARTESIAN_POINT('',(12.5609100301812,5.5,0.));
#21019=CARTESIAN_POINT('',(12.5609100301812,5.5,-1.1));
#21020=CARTESIAN_POINT('Origin',(12.7709100301812,5.5,0.));
#21021=CARTESIAN_POINT('Origin',(12.7709100301812,5.5,-1.1));
#21022=CARTESIAN_POINT('Origin',(12.7709100301812,2.5,-1.1));
#21023=CARTESIAN_POINT('',(12.5609100301812,2.5,-1.1));
#21024=CARTESIAN_POINT('Origin',(12.7709100301812,2.5,-1.1));
#21025=CARTESIAN_POINT('',(12.5609100301812,2.5,0.));
#21026=CARTESIAN_POINT('',(12.5609100301812,2.5,-1.1));
#21027=CARTESIAN_POINT('Origin',(12.7709100301812,2.5,0.));
#21028=CARTESIAN_POINT('Origin',(12.7709100301812,2.5,-1.1));
#21029=CARTESIAN_POINT('Origin',(1.17091003018116,5.5,-1.1));
#21030=CARTESIAN_POINT('',(0.960910030181156,5.5,-1.1));
#21031=CARTESIAN_POINT('Origin',(1.17091003018116,5.5,-1.1));
#21032=CARTESIAN_POINT('',(0.960910030181156,5.5,0.));
#21033=CARTESIAN_POINT('',(0.960910030181156,5.5,-1.1));
#21034=CARTESIAN_POINT('Origin',(1.17091003018116,5.5,0.));
#21035=CARTESIAN_POINT('Origin',(1.17091003018116,5.5,-1.1));
#21036=CARTESIAN_POINT('Origin',(1.17091003018116,2.5,-1.1));
#21037=CARTESIAN_POINT('',(0.960910030181156,2.5,-1.1));
#21038=CARTESIAN_POINT('Origin',(1.17091003018116,2.5,-1.1));
#21039=CARTESIAN_POINT('',(0.960910030181156,2.5,0.));
#21040=CARTESIAN_POINT('',(0.960910030181156,2.5,-1.1));
#21041=CARTESIAN_POINT('Origin',(1.17091003018116,2.5,0.));
#21042=CARTESIAN_POINT('Origin',(1.17091003018116,2.5,-1.1));
#21043=CARTESIAN_POINT('Origin',(8.77091003018116,1.,-1.3));
#21044=CARTESIAN_POINT('',(8.77091003018116,0.775,-1.2));
#21045=CARTESIAN_POINT('',(8.77091003018116,0.775,0.));
#21046=CARTESIAN_POINT('',(8.77091003018116,0.775,-1.3));
#21047=CARTESIAN_POINT('',(8.77091003018116,1.225,-1.2));
#21048=CARTESIAN_POINT('Origin',(8.77091003018116,1.,-1.2));
#21049=CARTESIAN_POINT('',(8.77091003018116,1.225,0.));
#21050=CARTESIAN_POINT('',(8.77091003018116,1.225,-1.3));
#21051=CARTESIAN_POINT('Origin',(8.77091003018116,1.,0.));
#21052=CARTESIAN_POINT('Origin',(10.7709100301812,1.,-1.3));
#21053=CARTESIAN_POINT('',(10.7709100301812,0.775,-1.2));
#21054=CARTESIAN_POINT('',(10.7709100301812,0.775,0.));
#21055=CARTESIAN_POINT('',(10.7709100301812,0.775,-1.3));
#21056=CARTESIAN_POINT('',(10.7709100301812,1.225,0.));
#21057=CARTESIAN_POINT('Origin',(10.7709100301812,1.,0.));
#21058=CARTESIAN_POINT('',(10.7709100301812,1.225,-1.2));
#21059=CARTESIAN_POINT('',(10.7709100301812,1.225,-1.3));
#21060=CARTESIAN_POINT('Origin',(10.7709100301812,1.,-1.2));
#21061=CARTESIAN_POINT('Origin',(5.25,19.,-1.2));
#21062=CARTESIAN_POINT('',(-4.,44.5,-1.2));
#21063=CARTESIAN_POINT('',(-4.,-6.5,-1.2));
#21064=CARTESIAN_POINT('',(-4.,44.5,-1.2));
#21065=CARTESIAN_POINT('',(14.5,44.5,-1.2));
#21066=CARTESIAN_POINT('',(14.5,44.5,-1.2));
#21067=CARTESIAN_POINT('',(14.5,-6.5,-1.2));
#21068=CARTESIAN_POINT('',(14.5,-6.5,-1.2));
#21069=CARTESIAN_POINT('',(-4.,-6.5,-1.2));
#21070=CARTESIAN_POINT('',(8.77091003018116,-0.775,-1.2));
#21071=CARTESIAN_POINT('',(8.77091003018116,-1.225,-1.2));
#21072=CARTESIAN_POINT('Origin',(8.77091003018116,-1.,-1.2));
#21073=CARTESIAN_POINT('',(10.7709100301812,-1.225,-1.2));
#21074=CARTESIAN_POINT('',(7.01045501509058,-1.225,-1.2));
#21075=CARTESIAN_POINT('',(10.7709100301812,-0.775,-1.2));
#21076=CARTESIAN_POINT('Origin',(10.7709100301812,-1.,-1.2));
#21077=CARTESIAN_POINT('',(8.01045501509058,-0.774999999999999,-1.2));
#21078=CARTESIAN_POINT('',(3.17091003018116,-0.775,-1.2));
#21079=CARTESIAN_POINT('',(3.17091003018116,-1.225,-1.2));
#21080=CARTESIAN_POINT('Origin',(3.17091003018116,-1.,-1.2));
#21081=CARTESIAN_POINT('',(5.17091003018116,-1.225,-1.2));
#21082=CARTESIAN_POINT('',(4.21045501509058,-1.225,-1.2));
#21083=CARTESIAN_POINT('',(5.17091003018116,-0.775,-1.2));
#21084=CARTESIAN_POINT('Origin',(5.17091003018116,-1.,-1.2));
#21085=CARTESIAN_POINT('',(5.21045501509058,-0.774999999999999,-1.2));
#21086=CARTESIAN_POINT('',(3.17091003018116,1.225,-1.2));
#21087=CARTESIAN_POINT('',(3.17091003018116,0.775,-1.2));
#21088=CARTESIAN_POINT('Origin',(3.17091003018116,1.,-1.2));
#21089=CARTESIAN_POINT('',(5.17091003018116,0.775,-1.2));
#21090=CARTESIAN_POINT('',(4.21045501509058,0.774999999999999,-1.2));
#21091=CARTESIAN_POINT('',(5.17091003018116,1.225,-1.2));
#21092=CARTESIAN_POINT('Origin',(5.17091003018116,1.,-1.2));
#21093=CARTESIAN_POINT('',(5.21045501509058,1.225,-1.2));
#21094=CARTESIAN_POINT('',(7.01045501509058,0.774999999999999,-1.2));
#21095=CARTESIAN_POINT('',(8.01045501509058,1.225,-1.2));
#21096=CARTESIAN_POINT('Origin',(10.7709100301812,1.225,-1.3));
#21097=CARTESIAN_POINT('',(8.01045501509058,1.225,0.));
#21098=CARTESIAN_POINT('Origin',(8.77091003018116,0.775,-1.3));
#21099=CARTESIAN_POINT('',(7.01045501509058,0.774999999999999,0.));
#21100=CARTESIAN_POINT('Origin',(8.77091003018116,-1.,-1.3));
#21101=CARTESIAN_POINT('',(8.77091003018116,-1.225,0.));
#21102=CARTESIAN_POINT('',(8.77091003018116,-1.225,-1.3));
#21103=CARTESIAN_POINT('',(8.77091003018116,-0.775,0.));
#21104=CARTESIAN_POINT('',(8.77091003018116,-0.775,-1.3));
#21105=CARTESIAN_POINT('Origin',(8.77091003018116,-1.,0.));
#21106=CARTESIAN_POINT('Origin',(10.7709100301812,-1.,-1.3));
#21107=CARTESIAN_POINT('',(10.7709100301812,-1.225,0.));
#21108=CARTESIAN_POINT('',(10.7709100301812,-1.225,-1.3));
#21109=CARTESIAN_POINT('',(10.7709100301812,-0.775,0.));
#21110=CARTESIAN_POINT('Origin',(10.7709100301812,-1.,0.));
#21111=CARTESIAN_POINT('',(10.7709100301812,-0.775,-1.3));
#21112=CARTESIAN_POINT('Origin',(10.7709100301812,-0.775,-1.3));
#21113=CARTESIAN_POINT('',(8.01045501509058,-0.774999999999999,0.));
#21114=CARTESIAN_POINT('Origin',(8.77091003018116,-1.225,-1.3));
#21115=CARTESIAN_POINT('',(7.01045501509058,-1.225,0.));
#21116=CARTESIAN_POINT('Origin',(3.17091003018116,1.,-1.3));
#21117=CARTESIAN_POINT('',(2.9539109773241,0.940532268757414,0.));
#21118=CARTESIAN_POINT('',(2.9539109773241,0.940532268757414,-1.1));
#21119=CARTESIAN_POINT('',(2.9539109773241,0.940532268757414,-1.3));
#21120=CARTESIAN_POINT('',(3.17091003018116,0.775,0.));
#21121=CARTESIAN_POINT('Origin',(3.17091003018116,1.,0.));
#21122=CARTESIAN_POINT('',(3.17091003018116,0.775,-1.3));
#21123=CARTESIAN_POINT('',(3.17091003018116,1.225,0.));
#21124=CARTESIAN_POINT('',(3.17091003018116,1.225,-1.3));
#21125=CARTESIAN_POINT('',(2.9539109773241,1.05946773124259,0.));
#21126=CARTESIAN_POINT('Origin',(3.17091003018116,1.,0.));
#21127=CARTESIAN_POINT('',(2.9539109773241,1.05946773124259,-1.1));
#21128=CARTESIAN_POINT('',(2.9539109773241,1.05946773124259,-1.3));
#21129=CARTESIAN_POINT('Origin',(3.17091003018116,1.,-1.1));
#21130=CARTESIAN_POINT('Origin',(5.17091003018116,1.,-1.3));
#21131=CARTESIAN_POINT('',(5.17091003018116,0.775,0.));
#21132=CARTESIAN_POINT('',(5.17091003018116,0.775,-1.3));
#21133=CARTESIAN_POINT('',(5.17091003018116,1.225,0.));
#21134=CARTESIAN_POINT('Origin',(5.17091003018116,1.,0.));
#21135=CARTESIAN_POINT('',(5.17091003018116,1.225,-1.3));
#21136=CARTESIAN_POINT('Origin',(5.17091003018116,1.225,-1.3));
#21137=CARTESIAN_POINT('',(5.21045501509058,1.225,0.));
#21138=CARTESIAN_POINT('Origin',(3.17091003018116,0.775,-1.3));
#21139=CARTESIAN_POINT('',(4.21045501509058,0.774999999999999,0.));
#21140=CARTESIAN_POINT('Origin',(3.17091003018116,-1.,-1.3));
#21141=CARTESIAN_POINT('',(2.9539109773241,-1.05946773124259,0.));
#21142=CARTESIAN_POINT('',(2.9539109773241,-1.05946773124259,-1.1));
#21143=CARTESIAN_POINT('',(2.9539109773241,-1.05946773124259,-1.3));
#21144=CARTESIAN_POINT('',(3.17091003018116,-1.225,0.));
#21145=CARTESIAN_POINT('Origin',(3.17091003018116,-1.,0.));
#21146=CARTESIAN_POINT('',(3.17091003018116,-1.225,-1.3));
#21147=CARTESIAN_POINT('',(3.17091003018116,-0.775,0.));
#21148=CARTESIAN_POINT('',(3.17091003018116,-0.775,-1.3));
#21149=CARTESIAN_POINT('',(2.9539109773241,-0.940532268757414,0.));
#21150=CARTESIAN_POINT('Origin',(3.17091003018116,-1.,0.));
#21151=CARTESIAN_POINT('',(2.9539109773241,-0.940532268757414,-1.1));
#21152=CARTESIAN_POINT('',(2.9539109773241,-0.940532268757414,-1.3));
#21153=CARTESIAN_POINT('Origin',(3.17091003018116,-1.,-1.1));
#21154=CARTESIAN_POINT('Origin',(5.17091003018116,-1.,-1.3));
#21155=CARTESIAN_POINT('',(5.17091003018116,-1.225,0.));
#21156=CARTESIAN_POINT('',(5.17091003018116,-1.225,-1.3));
#21157=CARTESIAN_POINT('',(5.17091003018116,-0.775,0.));
#21158=CARTESIAN_POINT('Origin',(5.17091003018116,-1.,0.));
#21159=CARTESIAN_POINT('',(5.17091003018116,-0.775,-1.3));
#21160=CARTESIAN_POINT('Origin',(5.17091003018116,-0.775,-1.3));
#21161=CARTESIAN_POINT('',(5.21045501509058,-0.774999999999999,0.));
#21162=CARTESIAN_POINT('Origin',(3.17091003018116,-1.225,-1.3));
#21163=CARTESIAN_POINT('',(4.21045501509058,-1.225,0.));
#21164=CARTESIAN_POINT('Origin',(2.8,-1.,-1.1));
#21165=CARTESIAN_POINT('Origin',(2.8,-1.,0.));
#21166=CARTESIAN_POINT('Origin',(2.8,-1.,-1.1));
#21167=CARTESIAN_POINT('Origin',(2.8,-1.,-1.1));
#21168=CARTESIAN_POINT('Origin',(-2.8,1.,-1.1));
#21169=CARTESIAN_POINT('',(-2.965,1.,-1.1));
#21170=CARTESIAN_POINT('Origin',(-2.8,1.,-1.1));
#21171=CARTESIAN_POINT('',(-2.965,1.,0.));
#21172=CARTESIAN_POINT('',(-2.965,1.,-1.1));
#21173=CARTESIAN_POINT('Origin',(-2.8,1.,0.));
#21174=CARTESIAN_POINT('Origin',(-2.8,1.,-1.1));
#21175=CARTESIAN_POINT('Origin',(-2.8,-1.,-1.1));
#21176=CARTESIAN_POINT('',(-2.965,-1.,-1.1));
#21177=CARTESIAN_POINT('Origin',(-2.8,-1.,-1.1));
#21178=CARTESIAN_POINT('',(-2.965,-1.,0.));
#21179=CARTESIAN_POINT('',(-2.965,-1.,-1.1));
#21180=CARTESIAN_POINT('Origin',(-2.8,-1.,0.));
#21181=CARTESIAN_POINT('Origin',(-2.8,-1.,-1.1));
#21182=CARTESIAN_POINT('Origin',(2.8,1.,-1.1));
#21183=CARTESIAN_POINT('Origin',(2.8,1.,0.));
#21184=CARTESIAN_POINT('Origin',(2.8,1.,-1.1));
#21185=CARTESIAN_POINT('Origin',(2.8,1.,-1.1));
#21186=CARTESIAN_POINT('Origin',(14.5,44.5,-1.2));
#21187=CARTESIAN_POINT('',(-4.,44.5,0.));
#21188=CARTESIAN_POINT('',(-4.,44.5,-1.2));
#21189=CARTESIAN_POINT('',(14.5,44.5,0.));
#21190=CARTESIAN_POINT('',(14.5,44.5,0.));
#21191=CARTESIAN_POINT('',(14.5,44.5,-1.2));
#21192=CARTESIAN_POINT('Origin',(14.5,-6.5,-1.2));
#21193=CARTESIAN_POINT('',(14.5,-6.5,0.));
#21194=CARTESIAN_POINT('',(14.5,-6.5,0.));
#21195=CARTESIAN_POINT('',(14.5,-6.5,-1.2));
#21196=CARTESIAN_POINT('Origin',(-4.,-6.5,-1.2));
#21197=CARTESIAN_POINT('',(-4.,-6.5,0.));
#21198=CARTESIAN_POINT('',(-4.,-6.5,0.));
#21199=CARTESIAN_POINT('',(-4.,-6.5,-1.2));
#21200=CARTESIAN_POINT('Origin',(-4.,44.5,-1.2));
#21201=CARTESIAN_POINT('',(-4.,44.5,0.));
#21202=CARTESIAN_POINT('Origin',(5.25,19.,0.));
#21203=CARTESIAN_POINT('',(0.,0.,0.));
#21204=CARTESIAN_POINT('Origin',(-3.,44.5,-2.4));
#21205=CARTESIAN_POINT('',(-3.,44.5,-2.4));
#21206=CARTESIAN_POINT('',(-4.,44.5,-2.4));
#21207=CARTESIAN_POINT('',(-3.,44.5,-2.4));
#21208=CARTESIAN_POINT('',(-4.,44.5,-1.2));
#21209=CARTESIAN_POINT('',(-4.,44.5,-2.4));
#21210=CARTESIAN_POINT('',(-3.,44.5,-1.2));
#21211=CARTESIAN_POINT('',(-3.,44.5,-1.2));
#21212=CARTESIAN_POINT('',(-3.,44.5,-2.4));
#21213=CARTESIAN_POINT('Origin',(-3.,-6.5,-2.4));
#21214=CARTESIAN_POINT('',(-3.,-6.5,-2.4));
#21215=CARTESIAN_POINT('',(-3.,-6.5,-2.4));
#21216=CARTESIAN_POINT('',(-3.,-6.5,-1.2));
#21217=CARTESIAN_POINT('',(-3.,-6.5,-1.2));
#21218=CARTESIAN_POINT('',(-3.,-6.5,-2.4));
#21219=CARTESIAN_POINT('Origin',(-4.,-6.5,-2.4));
#21220=CARTESIAN_POINT('',(-4.,-6.5,-2.4));
#21221=CARTESIAN_POINT('',(-4.,-6.5,-2.4));
#21222=CARTESIAN_POINT('',(-4.,-6.5,-1.2));
#21223=CARTESIAN_POINT('',(-4.,-6.5,-1.2));
#21224=CARTESIAN_POINT('',(-4.,-6.5,-2.4));
#21225=CARTESIAN_POINT('Origin',(-4.,44.5,-2.4));
#21226=CARTESIAN_POINT('',(-4.,44.5,-2.4));
#21227=CARTESIAN_POINT('',(-4.,44.5,-1.2));
#21228=CARTESIAN_POINT('Origin',(-3.5,19.,-1.2));
#21229=CARTESIAN_POINT('Origin',(-3.5,19.,-2.4));
#21230=CARTESIAN_POINT('',(0.,0.,0.));
#21231=CARTESIAN_POINT('Origin',(12.,44.5,-2.4));
#21232=CARTESIAN_POINT('',(12.,44.5,-2.4));
#21233=CARTESIAN_POINT('',(11.,44.5,-2.4));
#21234=CARTESIAN_POINT('',(12.,44.5,-2.4));
#21235=CARTESIAN_POINT('',(11.,44.5,-1.2));
#21236=CARTESIAN_POINT('',(11.,44.5,-2.4));
#21237=CARTESIAN_POINT('',(12.,44.5,-1.2));
#21238=CARTESIAN_POINT('',(12.,44.5,-1.2));
#21239=CARTESIAN_POINT('',(12.,44.5,-2.4));
#21240=CARTESIAN_POINT('Origin',(12.,-6.5,-2.4));
#21241=CARTESIAN_POINT('',(12.,-6.5,-2.4));
#21242=CARTESIAN_POINT('',(12.,-6.5,-2.4));
#21243=CARTESIAN_POINT('',(12.,-6.5,-1.2));
#21244=CARTESIAN_POINT('',(12.,-6.5,-1.2));
#21245=CARTESIAN_POINT('',(12.,-6.5,-2.4));
#21246=CARTESIAN_POINT('Origin',(11.,-6.5,-2.4));
#21247=CARTESIAN_POINT('',(11.,-6.5,-2.4));
#21248=CARTESIAN_POINT('',(11.,-6.5,-2.4));
#21249=CARTESIAN_POINT('',(11.,-6.5,-1.2));
#21250=CARTESIAN_POINT('',(11.,-6.5,-1.2));
#21251=CARTESIAN_POINT('',(11.,-6.5,-2.4));
#21252=CARTESIAN_POINT('Origin',(11.,44.5,-2.4));
#21253=CARTESIAN_POINT('',(11.,44.5,-2.4));
#21254=CARTESIAN_POINT('',(11.,44.5,-1.2));
#21255=CARTESIAN_POINT('Origin',(11.5,19.,-1.2));
#21256=CARTESIAN_POINT('Origin',(11.5,19.,-2.4));
#21257=CARTESIAN_POINT('',(0.,0.,0.));
#21258=CARTESIAN_POINT('Origin',(-1.34350288425444,-1.9,5.65649711574556));
#21259=CARTESIAN_POINT('',(-1.50850288425444,-1.8,5.65649711574556));
#21260=CARTESIAN_POINT('Origin',(-1.34350288425444,-1.8,5.65649711574556));
#21261=CARTESIAN_POINT('',(-1.50850288425444,1.8,5.65649711574556));
#21262=CARTESIAN_POINT('',(-1.50850288425444,-1.9,5.65649711574556));
#21263=CARTESIAN_POINT('Origin',(-1.34350288425444,1.8,5.65649711574556));
#21264=CARTESIAN_POINT('Origin',(-1.34350288425444,-1.9,8.34350288425444));
#21265=CARTESIAN_POINT('',(-1.50850288425444,-1.8,8.34350288425444));
#21266=CARTESIAN_POINT('Origin',(-1.34350288425444,-1.8,8.34350288425444));
#21267=CARTESIAN_POINT('',(-1.50850288425444,1.8,8.34350288425444));
#21268=CARTESIAN_POINT('',(-1.50850288425444,-1.9,8.34350288425444));
#21269=CARTESIAN_POINT('Origin',(-1.34350288425444,1.8,8.34350288425444));
#21270=CARTESIAN_POINT('Origin',(1.34350288425444,-1.9,8.34350288425444));
#21271=CARTESIAN_POINT('',(1.17850288425444,-1.8,8.34350288425444));
#21272=CARTESIAN_POINT('Origin',(1.34350288425444,-1.8,8.34350288425444));
#21273=CARTESIAN_POINT('',(1.17850288425444,1.8,8.34350288425444));
#21274=CARTESIAN_POINT('',(1.17850288425444,-1.9,8.34350288425444));
#21275=CARTESIAN_POINT('Origin',(1.34350288425444,1.8,8.34350288425444));
#21276=CARTESIAN_POINT('Origin',(1.34350288425444,-1.9,5.65649711574556));
#21277=CARTESIAN_POINT('',(1.17850288425444,-1.8,5.65649711574556));
#21278=CARTESIAN_POINT('Origin',(1.34350288425444,-1.8,5.65649711574556));
#21279=CARTESIAN_POINT('',(1.17850288425444,1.8,5.65649711574556));
#21280=CARTESIAN_POINT('',(1.17850288425444,-1.9,5.65649711574556));
#21281=CARTESIAN_POINT('Origin',(1.34350288425444,1.8,5.65649711574556));
#21282=CARTESIAN_POINT('Origin',(0.,-1.9,7.));
#21283=CARTESIAN_POINT('',(-1.5,-1.8,7.));
#21284=CARTESIAN_POINT('Origin',(0.,-1.8,7.));
#21285=CARTESIAN_POINT('',(-1.5,1.8,7.));
#21286=CARTESIAN_POINT('',(-1.5,-1.9,7.));
#21287=CARTESIAN_POINT('Origin',(0.,1.8,7.));
#21288=CARTESIAN_POINT('Origin',(2.8,-1.,-0.1));
#21289=CARTESIAN_POINT('',(2.575,-1.,0.));
#21290=CARTESIAN_POINT('Origin',(2.8,-1.,0.));
#21291=CARTESIAN_POINT('',(2.575,-1.,0.8));
#21292=CARTESIAN_POINT('',(2.575,-1.,-0.1));
#21293=CARTESIAN_POINT('Origin',(2.8,-1.,0.8));
#21294=CARTESIAN_POINT('Origin',(-2.8,1.,-0.1));
#21295=CARTESIAN_POINT('',(-3.025,1.,0.));
#21296=CARTESIAN_POINT('Origin',(-2.8,1.,0.));
#21297=CARTESIAN_POINT('',(-3.025,1.,0.8));
#21298=CARTESIAN_POINT('',(-3.025,1.,-0.1));
#21299=CARTESIAN_POINT('Origin',(-2.8,1.,0.8));
#21300=CARTESIAN_POINT('Origin',(-2.8,-1.,-0.1));
#21301=CARTESIAN_POINT('',(-3.025,-1.,0.));
#21302=CARTESIAN_POINT('Origin',(-2.8,-1.,0.));
#21303=CARTESIAN_POINT('',(-3.025,-1.,0.8));
#21304=CARTESIAN_POINT('',(-3.025,-1.,-0.1));
#21305=CARTESIAN_POINT('Origin',(-2.8,-1.,0.8));
#21306=CARTESIAN_POINT('Origin',(2.8,1.,-0.1));
#21307=CARTESIAN_POINT('',(2.575,1.,0.));
#21308=CARTESIAN_POINT('Origin',(2.8,1.,0.));
#21309=CARTESIAN_POINT('',(2.575,1.,0.8));
#21310=CARTESIAN_POINT('',(2.575,1.,-0.1));
#21311=CARTESIAN_POINT('Origin',(2.8,1.,0.8));
#21312=CARTESIAN_POINT('Origin',(-3.4,-1.8,0.8));
#21313=CARTESIAN_POINT('',(2.2,-1.8,0.8));
#21314=CARTESIAN_POINT('',(2.2,1.8,0.8));
#21315=CARTESIAN_POINT('',(2.2,-1.8,0.8));
#21316=CARTESIAN_POINT('',(3.4,-1.8,0.8));
#21317=CARTESIAN_POINT('',(3.4,-1.8,0.8));
#21318=CARTESIAN_POINT('',(3.4,1.8,0.8));
#21319=CARTESIAN_POINT('',(3.4,-1.8,0.8));
#21320=CARTESIAN_POINT('',(3.4,1.8,0.8));
#21321=CARTESIAN_POINT('Origin',(-3.4,-1.8,0.8));
#21322=CARTESIAN_POINT('',(-2.2,1.8,0.8));
#21323=CARTESIAN_POINT('',(-2.2,-1.8,0.8));
#21324=CARTESIAN_POINT('',(-2.2,0.,0.8));
#21325=CARTESIAN_POINT('',(-3.4,1.8,0.8));
#21326=CARTESIAN_POINT('',(3.4,1.8,0.8));
#21327=CARTESIAN_POINT('',(-3.4,-1.8,0.8));
#21328=CARTESIAN_POINT('',(-3.4,-1.8,0.8));
#21329=CARTESIAN_POINT('',(3.4,-1.8,0.8));
#21330=CARTESIAN_POINT('Origin',(-3.4,-1.8,0.));
#21331=CARTESIAN_POINT('',(-3.4,-1.8,0.));
#21332=CARTESIAN_POINT('',(-3.4,-1.8,0.8));
#21333=CARTESIAN_POINT('',(-3.4,1.8,0.));
#21334=CARTESIAN_POINT('',(-3.4,1.8,0.8));
#21335=CARTESIAN_POINT('',(-3.4,-1.8,0.));
#21336=CARTESIAN_POINT('Origin',(3.4,-1.8,0.8));
#21337=CARTESIAN_POINT('',(3.4,-1.8,0.));
#21338=CARTESIAN_POINT('',(3.4,-1.8,0.));
#21339=CARTESIAN_POINT('',(3.4,1.8,0.));
#21340=CARTESIAN_POINT('',(3.4,-1.8,0.));
#21341=CARTESIAN_POINT('',(3.4,1.8,0.));
#21342=CARTESIAN_POINT('Origin',(-2.2,-1.8,0.));
#21343=CARTESIAN_POINT('',(2.2,-1.8,9.2));
#21344=CARTESIAN_POINT('',(2.2,-1.8,0.));
#21345=CARTESIAN_POINT('',(-2.2,-1.8,9.2));
#21346=CARTESIAN_POINT('',(-2.2,-1.8,9.2));
#21347=CARTESIAN_POINT('',(-2.2,-1.8,0.));
#21348=CARTESIAN_POINT('',(-3.4,-1.8,0.));
#21349=CARTESIAN_POINT('Origin',(2.2,-1.8,0.));
#21350=CARTESIAN_POINT('',(2.2,1.8,9.2));
#21351=CARTESIAN_POINT('',(2.2,1.8,0.));
#21352=CARTESIAN_POINT('',(2.2,-1.8,9.2));
#21353=CARTESIAN_POINT('Origin',(2.2,1.8,0.));
#21354=CARTESIAN_POINT('',(-2.2,1.8,9.2));
#21355=CARTESIAN_POINT('',(-2.2,1.8,0.));
#21356=CARTESIAN_POINT('',(2.2,1.8,9.2));
#21357=CARTESIAN_POINT('',(-3.4,1.8,0.));
#21358=CARTESIAN_POINT('Origin',(-2.2,1.8,0.));
#21359=CARTESIAN_POINT('',(-2.2,1.8,9.2));
#21360=CARTESIAN_POINT('Origin',(0.,0.,9.2));
#21361=CARTESIAN_POINT('Origin',(0.,0.,0.));
#21362=CARTESIAN_POINT('',(0.,0.,0.));
#21363=CARTESIAN_POINT('Origin',(0.,-0.45,7.));
#21364=CARTESIAN_POINT('',(-1.1,0.45,7.));
#21365=CARTESIAN_POINT('Origin',(0.,0.45,7.));
#21366=CARTESIAN_POINT('',(-1.1,-0.45,7.));
#21367=CARTESIAN_POINT('',(-1.1,-0.45,7.));
#21368=CARTESIAN_POINT('Origin',(0.,-0.45,7.));
#21369=CARTESIAN_POINT('Origin',(0.,-0.45,7.));
#21370=CARTESIAN_POINT('',(-1.49,0.45,7.));
#21371=CARTESIAN_POINT('Origin',(0.,0.45,7.));
#21372=CARTESIAN_POINT('',(-1.49,-0.45,7.));
#21373=CARTESIAN_POINT('',(-1.49,-0.45,7.));
#21374=CARTESIAN_POINT('Origin',(0.,-0.45,7.));
#21375=CARTESIAN_POINT('Origin',(0.,0.45,7.));
#21376=CARTESIAN_POINT('Origin',(0.,-0.45,7.));
#21377=CARTESIAN_POINT('',(0.,0.,0.));
#21378=CARTESIAN_POINT('Origin',(-1.34350288425444,-2.2,5.65649711574556));
#21379=CARTESIAN_POINT('',(-1.40634555589641,-2.1,5.4404512904656));
#21380=CARTESIAN_POINT('',(-1.40634555589641,-1.8,5.4404512904656));
#21381=CARTESIAN_POINT('',(-1.40634555589641,-2.2,5.4404512904656));
#21382=CARTESIAN_POINT('',(-1.5595487095344,-2.1,5.59365444410359));
#21383=CARTESIAN_POINT('Origin',(-1.34350288425444,-2.1,5.65649711574556));
#21384=CARTESIAN_POINT('',(-1.5595487095344,-1.8,5.59365444410359));
#21385=CARTESIAN_POINT('',(-1.5595487095344,-2.2,5.59365444410359));
#21386=CARTESIAN_POINT('Origin',(-1.34350288425444,-1.8,5.65649711574556));
#21387=CARTESIAN_POINT('Origin',(-1.34350288425444,-2.2,8.34350288425444));
#21388=CARTESIAN_POINT('',(-1.5595487095344,-2.1,8.40634555589641));
#21389=CARTESIAN_POINT('',(-1.5595487095344,-1.8,8.40634555589641));
#21390=CARTESIAN_POINT('',(-1.5595487095344,-2.2,8.40634555589641));
#21391=CARTESIAN_POINT('',(-1.40634555589641,-2.1,8.5595487095344));
#21392=CARTESIAN_POINT('Origin',(-1.34350288425444,-2.1,8.34350288425444));
#21393=CARTESIAN_POINT('',(-1.40634555589641,-1.8,8.5595487095344));
#21394=CARTESIAN_POINT('',(-1.40634555589641,-2.2,8.5595487095344));
#21395=CARTESIAN_POINT('Origin',(-1.34350288425444,-1.8,8.34350288425444));
#21396=CARTESIAN_POINT('Origin',(1.34350288425444,-2.2,8.34350288425444));
#21397=CARTESIAN_POINT('',(1.40634555589641,-2.1,8.5595487095344));
#21398=CARTESIAN_POINT('',(1.40634555589641,-1.8,8.5595487095344));
#21399=CARTESIAN_POINT('',(1.40634555589641,-2.2,8.5595487095344));
#21400=CARTESIAN_POINT('',(1.5595487095344,-2.1,8.40634555589641));
#21401=CARTESIAN_POINT('Origin',(1.34350288425444,-2.1,8.34350288425444));
#21402=CARTESIAN_POINT('',(1.5595487095344,-1.8,8.40634555589641));
#21403=CARTESIAN_POINT('',(1.5595487095344,-2.2,8.40634555589641));
#21404=CARTESIAN_POINT('Origin',(1.34350288425444,-1.8,8.34350288425444));
#21405=CARTESIAN_POINT('Origin',(1.34350288425444,-2.2,5.65649711574556));
#21406=CARTESIAN_POINT('',(1.5595487095344,-2.1,5.59365444410359));
#21407=CARTESIAN_POINT('',(1.5595487095344,-1.8,5.59365444410359));
#21408=CARTESIAN_POINT('',(1.5595487095344,-2.2,5.59365444410359));
#21409=CARTESIAN_POINT('',(1.40634555589641,-2.1,5.4404512904656));
#21410=CARTESIAN_POINT('Origin',(1.34350288425444,-2.1,5.65649711574556));
#21411=CARTESIAN_POINT('',(1.40634555589641,-1.8,5.4404512904656));
#21412=CARTESIAN_POINT('',(1.40634555589641,-2.2,5.4404512904656));
#21413=CARTESIAN_POINT('Origin',(1.34350288425444,-1.8,5.65649711574556));
#21414=CARTESIAN_POINT('Origin',(0.,-2.1,7.));
#21415=CARTESIAN_POINT('Origin',(0.,-2.1,7.));
#21416=CARTESIAN_POINT('Origin',(0.,-2.1,7.));
#21417=CARTESIAN_POINT('Origin',(0.,-2.1,7.));
#21418=CARTESIAN_POINT('Origin',(0.,-2.1,7.));
#21419=CARTESIAN_POINT('',(-1.1,-2.1,7.));
#21420=CARTESIAN_POINT('Origin',(0.,-2.1,7.));
#21421=CARTESIAN_POINT('Origin',(0.,-2.1,7.));
#21422=CARTESIAN_POINT('Origin',(0.,-1.8,7.));
#21423=CARTESIAN_POINT('Origin',(0.,-2.1,7.));
#21424=CARTESIAN_POINT('Origin',(0.,-1.8,7.));
#21425=CARTESIAN_POINT('Origin',(0.,-2.1,7.));
#21426=CARTESIAN_POINT('Origin',(0.,-1.8,7.));
#21427=CARTESIAN_POINT('Origin',(0.,-2.1,7.));
#21428=CARTESIAN_POINT('Origin',(0.,-1.8,7.));
#21429=CARTESIAN_POINT('Origin',(0.,-1.8,7.));
#21430=CARTESIAN_POINT('',(-1.49,-1.35,7.));
#21431=CARTESIAN_POINT('Origin',(0.,-1.35,7.));
#21432=CARTESIAN_POINT('',(-1.49,-1.8,7.));
#21433=CARTESIAN_POINT('',(-1.49,-1.8,7.));
#21434=CARTESIAN_POINT('Origin',(0.,-1.8,7.));
#21435=CARTESIAN_POINT('Origin',(0.,-1.35,7.));
#21436=CARTESIAN_POINT('',(-1.1,-1.35,7.));
#21437=CARTESIAN_POINT('Origin',(0.,-1.35,7.));
#21438=CARTESIAN_POINT('Origin',(0.,-2.1,7.));
#21439=CARTESIAN_POINT('',(-1.1,-2.1,7.));
#21440=CARTESIAN_POINT('Origin',(0.,-1.8,7.));
#21441=CARTESIAN_POINT('',(0.,0.,0.));
#21442=CARTESIAN_POINT('Origin',(-1.34350288425444,1.7,5.65649711574556));
#21443=CARTESIAN_POINT('',(-1.40634555589641,1.8,5.4404512904656));
#21444=CARTESIAN_POINT('',(-1.40634555589641,2.1,5.4404512904656));
#21445=CARTESIAN_POINT('',(-1.40634555589641,1.7,5.4404512904656));
#21446=CARTESIAN_POINT('',(-1.5595487095344,1.8,5.59365444410359));
#21447=CARTESIAN_POINT('Origin',(-1.34350288425444,1.8,5.65649711574556));
#21448=CARTESIAN_POINT('',(-1.5595487095344,2.1,5.59365444410359));
#21449=CARTESIAN_POINT('',(-1.5595487095344,1.7,5.59365444410359));
#21450=CARTESIAN_POINT('Origin',(-1.34350288425444,2.1,5.65649711574556));
#21451=CARTESIAN_POINT('Origin',(-1.34350288425444,1.7,8.34350288425444));
#21452=CARTESIAN_POINT('',(-1.5595487095344,1.8,8.40634555589641));
#21453=CARTESIAN_POINT('',(-1.5595487095344,2.1,8.40634555589641));
#21454=CARTESIAN_POINT('',(-1.5595487095344,1.7,8.40634555589641));
#21455=CARTESIAN_POINT('',(-1.40634555589641,1.8,8.5595487095344));
#21456=CARTESIAN_POINT('Origin',(-1.34350288425444,1.8,8.34350288425444));
#21457=CARTESIAN_POINT('',(-1.40634555589641,2.1,8.5595487095344));
#21458=CARTESIAN_POINT('',(-1.40634555589641,1.7,8.5595487095344));
#21459=CARTESIAN_POINT('Origin',(-1.34350288425444,2.1,8.34350288425444));
#21460=CARTESIAN_POINT('Origin',(1.34350288425444,1.7,8.34350288425444));
#21461=CARTESIAN_POINT('',(1.40634555589641,1.8,8.5595487095344));
#21462=CARTESIAN_POINT('',(1.40634555589641,2.1,8.5595487095344));
#21463=CARTESIAN_POINT('',(1.40634555589641,1.7,8.5595487095344));
#21464=CARTESIAN_POINT('',(1.5595487095344,1.8,8.40634555589641));
#21465=CARTESIAN_POINT('Origin',(1.34350288425444,1.8,8.34350288425444));
#21466=CARTESIAN_POINT('',(1.5595487095344,2.1,8.40634555589641));
#21467=CARTESIAN_POINT('',(1.5595487095344,1.7,8.40634555589641));
#21468=CARTESIAN_POINT('Origin',(1.34350288425444,2.1,8.34350288425444));
#21469=CARTESIAN_POINT('Origin',(1.34350288425444,1.7,5.65649711574556));
#21470=CARTESIAN_POINT('',(1.5595487095344,1.8,5.59365444410359));
#21471=CARTESIAN_POINT('',(1.5595487095344,2.1,5.59365444410359));
#21472=CARTESIAN_POINT('',(1.5595487095344,1.7,5.59365444410359));
#21473=CARTESIAN_POINT('',(1.40634555589641,1.8,5.4404512904656));
#21474=CARTESIAN_POINT('Origin',(1.34350288425444,1.8,5.65649711574556));
#21475=CARTESIAN_POINT('',(1.40634555589641,2.1,5.4404512904656));
#21476=CARTESIAN_POINT('',(1.40634555589641,1.7,5.4404512904656));
#21477=CARTESIAN_POINT('Origin',(1.34350288425444,2.1,5.65649711574556));
#21478=CARTESIAN_POINT('Origin',(0.,1.8,7.));
#21479=CARTESIAN_POINT('Origin',(0.,1.8,7.));
#21480=CARTESIAN_POINT('Origin',(0.,1.8,7.));
#21481=CARTESIAN_POINT('Origin',(0.,1.8,7.));
#21482=CARTESIAN_POINT('Origin',(0.,1.8,7.));
#21483=CARTESIAN_POINT('',(-1.49,1.8,7.));
#21484=CARTESIAN_POINT('Origin',(0.,1.8,7.));
#21485=CARTESIAN_POINT('Origin',(0.,1.8,7.));
#21486=CARTESIAN_POINT('Origin',(0.,2.1,7.));
#21487=CARTESIAN_POINT('Origin',(0.,1.8,7.));
#21488=CARTESIAN_POINT('Origin',(0.,2.1,7.));
#21489=CARTESIAN_POINT('Origin',(0.,1.8,7.));
#21490=CARTESIAN_POINT('Origin',(0.,2.1,7.));
#21491=CARTESIAN_POINT('Origin',(0.,1.8,7.));
#21492=CARTESIAN_POINT('Origin',(0.,2.1,7.));
#21493=CARTESIAN_POINT('Origin',(0.,1.35,7.));
#21494=CARTESIAN_POINT('',(-1.49,1.35,7.));
#21495=CARTESIAN_POINT('',(-1.49,1.35,7.));
#21496=CARTESIAN_POINT('Origin',(0.,1.35,7.));
#21497=CARTESIAN_POINT('Origin',(0.,1.35,7.));
#21498=CARTESIAN_POINT('',(-1.1,1.35,7.));
#21499=CARTESIAN_POINT('Origin',(0.,1.35,7.));
#21500=CARTESIAN_POINT('Origin',(0.,1.8,7.));
#21501=CARTESIAN_POINT('',(-1.1,2.1,7.));
#21502=CARTESIAN_POINT('Origin',(0.,2.1,7.));
#21503=CARTESIAN_POINT('',(-1.1,1.8,7.));
#21504=CARTESIAN_POINT('Origin',(0.,2.1,7.));
#21505=CARTESIAN_POINT('',(0.,0.,0.));
#21506=CARTESIAN_POINT('Origin',(6.97091003018116,1.4,7.));
#21507=CARTESIAN_POINT('',(9.17091003018116,1.4,7.21));
#21508=CARTESIAN_POINT('',(9.17091003018116,1.8,7.21));
#21509=CARTESIAN_POINT('',(9.17091003018116,1.4,7.21));
#21510=CARTESIAN_POINT('',(7.18091003018115,1.4,9.2));
#21511=CARTESIAN_POINT('Origin',(6.97091003018116,1.4,7.));
#21512=CARTESIAN_POINT('',(7.18091003018115,1.8,9.2));
#21513=CARTESIAN_POINT('',(7.18091003018115,1.4,9.2));
#21514=CARTESIAN_POINT('Origin',(6.97091003018116,1.8,7.));
#21515=CARTESIAN_POINT('Origin',(6.97091003018116,1.4,7.));
#21516=CARTESIAN_POINT('',(4.77091003018116,1.8,7.21));
#21517=CARTESIAN_POINT('',(4.77091003018116,1.4,7.21));
#21518=CARTESIAN_POINT('',(4.77091003018116,1.4,7.21));
#21519=CARTESIAN_POINT('',(6.76091003018117,1.8,9.2));
#21520=CARTESIAN_POINT('Origin',(6.97091003018116,1.8,7.));
#21521=CARTESIAN_POINT('',(6.76091003018117,1.4,9.2));
#21522=CARTESIAN_POINT('',(6.76091003018117,1.4,9.2));
#21523=CARTESIAN_POINT('Origin',(6.97091003018116,1.4,7.));
#21524=CARTESIAN_POINT('Origin',(6.97091003018116,1.4,7.));
#21525=CARTESIAN_POINT('',(9.17091003018116,1.4,6.79));
#21526=CARTESIAN_POINT('',(9.17091003018116,1.4,3.5));
#21527=CARTESIAN_POINT('',(4.77091003018116,1.4,6.79));
#21528=CARTESIAN_POINT('Origin',(6.97091003018116,1.4,7.));
#21529=CARTESIAN_POINT('',(4.77091003018116,1.4,3.5));
#21530=CARTESIAN_POINT('',(6.97091003018116,1.4,9.2));
#21531=CARTESIAN_POINT('',(5.37091003018116,1.4,7.));
#21532=CARTESIAN_POINT('Origin',(6.97091003018116,1.4,7.));
#21533=CARTESIAN_POINT('',(8.22012359255425,1.4,5.58578643762691));
#21534=CARTESIAN_POINT('Origin',(8.38512359255425,1.4,5.58578643762691));
#21535=CARTESIAN_POINT('',(8.22012359255425,1.4,8.4142135623731));
#21536=CARTESIAN_POINT('Origin',(8.38512359255425,1.4,8.4142135623731));
#21537=CARTESIAN_POINT('',(5.39169646780806,1.4,8.4142135623731));
#21538=CARTESIAN_POINT('Origin',(5.55669646780806,1.4,8.4142135623731));
#21539=CARTESIAN_POINT('',(5.39169646780806,1.4,5.58578643762691));
#21540=CARTESIAN_POINT('Origin',(5.55669646780806,1.4,5.58578643762691));
#21541=CARTESIAN_POINT('Origin',(6.97091003018116,1.4,7.));
#21542=CARTESIAN_POINT('',(9.17091003018116,1.8,6.79));
#21543=CARTESIAN_POINT('',(9.17091003018116,1.4,6.79));
#21544=CARTESIAN_POINT('',(4.77091003018116,1.8,6.79));
#21545=CARTESIAN_POINT('Origin',(6.97091003018116,1.8,7.));
#21546=CARTESIAN_POINT('',(4.77091003018116,1.4,6.79));
#21547=CARTESIAN_POINT('Origin',(9.17091003018116,-1.8,0.));
#21548=CARTESIAN_POINT('',(9.17091003018116,1.8,9.2));
#21549=CARTESIAN_POINT('',(9.17091003018116,1.8,0.));
#21550=CARTESIAN_POINT('',(9.17091003018116,-1.8,9.2));
#21551=CARTESIAN_POINT('',(9.17091003018116,-1.8,9.2));
#21552=CARTESIAN_POINT('',(9.17091003018116,-1.8,0.8));
#21553=CARTESIAN_POINT('',(9.17091003018116,-1.8,0.));
#21554=CARTESIAN_POINT('',(9.17091003018116,1.8,0.8));
#21555=CARTESIAN_POINT('',(9.17091003018116,-1.8,0.8));
#21556=CARTESIAN_POINT('',(9.17091003018116,1.8,0.));
#21557=CARTESIAN_POINT('Origin',(6.97091003018116,0.,9.2));
#21558=CARTESIAN_POINT('',(4.77091003018116,1.8,9.2));
#21559=CARTESIAN_POINT('',(9.17091003018116,1.8,9.2));
#21560=CARTESIAN_POINT('',(4.77091003018116,-1.8,9.2));
#21561=CARTESIAN_POINT('',(4.77091003018116,1.8,9.2));
#21562=CARTESIAN_POINT('',(4.77091003018116,-1.8,9.2));
#21563=CARTESIAN_POINT('',(9.17091003018116,1.8,9.2));
#21564=CARTESIAN_POINT('Origin',(9.17091003018116,1.8,0.));
#21565=CARTESIAN_POINT('Origin',(9.17091003018116,1.8,0.));
#21566=CARTESIAN_POINT('',(4.77091003018116,1.8,0.));
#21567=CARTESIAN_POINT('Origin',(5.55669646780806,-1.9,5.58578643762691));
#21568=CARTESIAN_POINT('',(5.39169646780806,-1.8,5.58578643762691));
#21569=CARTESIAN_POINT('Origin',(5.55669646780806,-1.8,5.58578643762691));
#21570=CARTESIAN_POINT('',(5.39169646780806,-1.9,5.58578643762691));
#21571=CARTESIAN_POINT('Origin',(5.55669646780806,-1.9,8.4142135623731));
#21572=CARTESIAN_POINT('',(5.39169646780806,-1.8,8.4142135623731));
#21573=CARTESIAN_POINT('Origin',(5.55669646780806,-1.8,8.4142135623731));
#21574=CARTESIAN_POINT('',(5.39169646780806,-1.9,8.4142135623731));
#21575=CARTESIAN_POINT('Origin',(8.38512359255425,-1.9,8.4142135623731));
#21576=CARTESIAN_POINT('',(8.22012359255425,-1.8,8.4142135623731));
#21577=CARTESIAN_POINT('Origin',(8.38512359255425,-1.8,8.4142135623731));
#21578=CARTESIAN_POINT('',(8.22012359255425,-1.9,8.4142135623731));
#21579=CARTESIAN_POINT('Origin',(8.38512359255425,-1.9,5.58578643762691));
#21580=CARTESIAN_POINT('',(8.22012359255425,-1.8,5.58578643762691));
#21581=CARTESIAN_POINT('Origin',(8.38512359255425,-1.8,5.58578643762691));
#21582=CARTESIAN_POINT('',(8.22012359255425,-1.9,5.58578643762691));
#21583=CARTESIAN_POINT('Origin',(6.97091003018116,-1.9,7.));
#21584=CARTESIAN_POINT('',(5.37091003018116,-1.8,7.));
#21585=CARTESIAN_POINT('Origin',(6.97091003018116,-1.8,7.));
#21586=CARTESIAN_POINT('',(5.37091003018116,-1.9,7.));
#21587=CARTESIAN_POINT('Origin',(9.77091003018116,-1.,-0.1));
#21588=CARTESIAN_POINT('',(9.54591003018116,-1.,0.));
#21589=CARTESIAN_POINT('Origin',(9.77091003018116,-1.,0.));
#21590=CARTESIAN_POINT('',(9.54591003018116,-1.,0.8));
#21591=CARTESIAN_POINT('',(9.54591003018116,-1.,-0.1));
#21592=CARTESIAN_POINT('Origin',(9.77091003018116,-1.,0.8));
#21593=CARTESIAN_POINT('Origin',(4.17091003018116,1.,-0.1));
#21594=CARTESIAN_POINT('',(3.94591003018116,1.,0.));
#21595=CARTESIAN_POINT('Origin',(4.17091003018116,1.,0.));
#21596=CARTESIAN_POINT('',(3.94591003018116,1.,0.8));
#21597=CARTESIAN_POINT('',(3.94591003018116,1.,-0.1));
#21598=CARTESIAN_POINT('Origin',(4.17091003018116,1.,0.8));
#21599=CARTESIAN_POINT('Origin',(4.17091003018116,-1.,-0.1));
#21600=CARTESIAN_POINT('',(3.94591003018116,-1.,0.));
#21601=CARTESIAN_POINT('Origin',(4.17091003018116,-1.,0.));
#21602=CARTESIAN_POINT('',(3.94591003018116,-1.,0.8));
#21603=CARTESIAN_POINT('',(3.94591003018116,-1.,-0.1));
#21604=CARTESIAN_POINT('Origin',(4.17091003018116,-1.,0.8));
#21605=CARTESIAN_POINT('Origin',(9.77091003018116,1.,-0.1));
#21606=CARTESIAN_POINT('',(9.54591003018116,1.,0.));
#21607=CARTESIAN_POINT('Origin',(9.77091003018116,1.,0.));
#21608=CARTESIAN_POINT('',(9.54591003018116,1.,0.8));
#21609=CARTESIAN_POINT('',(9.54591003018116,1.,-0.1));
#21610=CARTESIAN_POINT('Origin',(9.77091003018116,1.,0.8));
#21611=CARTESIAN_POINT('Origin',(3.57091003018116,-1.8,0.8));
#21612=CARTESIAN_POINT('',(10.3709100301812,-1.8,0.8));
#21613=CARTESIAN_POINT('',(10.3709100301812,-1.8,0.8));
#21614=CARTESIAN_POINT('',(10.3709100301812,1.8,0.8));
#21615=CARTESIAN_POINT('',(10.3709100301812,-1.8,0.8));
#21616=CARTESIAN_POINT('',(10.3709100301812,1.8,0.8));
#21617=CARTESIAN_POINT('Origin',(3.57091003018116,-1.8,0.8));
#21618=CARTESIAN_POINT('',(4.77091003018116,1.8,0.8));
#21619=CARTESIAN_POINT('',(4.77091003018116,-1.8,0.8));
#21620=CARTESIAN_POINT('',(4.77091003018116,0.,0.8));
#21621=CARTESIAN_POINT('',(3.57091003018116,1.8,0.8));
#21622=CARTESIAN_POINT('',(10.3709100301812,1.8,0.8));
#21623=CARTESIAN_POINT('',(3.57091003018116,-1.8,0.8));
#21624=CARTESIAN_POINT('',(3.57091003018116,-1.8,0.8));
#21625=CARTESIAN_POINT('',(10.3709100301812,-1.8,0.8));
#21626=CARTESIAN_POINT('Origin',(3.57091003018116,-1.8,0.));
#21627=CARTESIAN_POINT('',(3.57091003018116,-1.8,0.));
#21628=CARTESIAN_POINT('',(3.57091003018116,-1.8,0.8));
#21629=CARTESIAN_POINT('',(3.57091003018116,1.8,0.));
#21630=CARTESIAN_POINT('',(3.57091003018116,1.8,0.8));
#21631=CARTESIAN_POINT('',(3.57091003018116,-1.8,0.));
#21632=CARTESIAN_POINT('Origin',(10.3709100301812,-1.8,0.8));
#21633=CARTESIAN_POINT('',(10.3709100301812,-1.8,0.));
#21634=CARTESIAN_POINT('',(10.3709100301812,-1.8,0.));
#21635=CARTESIAN_POINT('',(10.3709100301812,1.8,0.));
#21636=CARTESIAN_POINT('',(10.3709100301812,-1.8,0.));
#21637=CARTESIAN_POINT('',(10.3709100301812,1.8,0.));
#21638=CARTESIAN_POINT('Origin',(4.77091003018116,-1.8,0.));
#21639=CARTESIAN_POINT('',(4.77091003018116,-1.8,0.));
#21640=CARTESIAN_POINT('',(3.57091003018116,-1.8,0.));
#21641=CARTESIAN_POINT('Origin',(9.17091003018116,1.8,0.));
#21642=CARTESIAN_POINT('',(3.57091003018116,1.8,0.));
#21643=CARTESIAN_POINT('',(4.77091003018116,1.8,0.));
#21644=CARTESIAN_POINT('Origin',(4.77091003018116,1.8,0.));
#21645=CARTESIAN_POINT('Origin',(6.97091003018116,0.,0.));
#21646=CARTESIAN_POINT('',(0.,0.,0.));
#21647=CARTESIAN_POINT('Origin',(4.17091003018116,-1.,-1.6));
#21648=CARTESIAN_POINT('',(4.00591003018116,-1.,-1.2));
#21649=CARTESIAN_POINT('Origin',(4.17091003018116,-1.,-1.2));
#21650=CARTESIAN_POINT('',(4.00591003018116,-1.,-1.6));
#21651=CARTESIAN_POINT('',(4.00591003018116,-1.,-1.6));
#21652=CARTESIAN_POINT('Origin',(4.17091003018116,-1.,-1.6));
#21653=CARTESIAN_POINT('Origin',(4.17091003018116,-1.,-1.6));
#21654=CARTESIAN_POINT('',(3.77091003018116,-1.,-1.2));
#21655=CARTESIAN_POINT('Origin',(4.17091003018116,-1.,-1.2));
#21656=CARTESIAN_POINT('',(3.77091003018116,-1.,-1.6));
#21657=CARTESIAN_POINT('',(3.77091003018116,-1.,-1.6));
#21658=CARTESIAN_POINT('Origin',(4.17091003018116,-1.,-1.6));
#21659=CARTESIAN_POINT('Origin',(4.17091003018116,-1.,-1.2));
#21660=CARTESIAN_POINT('Origin',(4.17091003018116,-1.,-1.6));
#21661=CARTESIAN_POINT('',(0.,0.,0.));
#21662=CARTESIAN_POINT('Origin',(4.17091003018116,1.,-1.6));
#21663=CARTESIAN_POINT('',(4.00591003018116,1.,-1.2));
#21664=CARTESIAN_POINT('Origin',(4.17091003018116,1.,-1.2));
#21665=CARTESIAN_POINT('',(4.00591003018116,1.,-1.6));
#21666=CARTESIAN_POINT('',(4.00591003018116,1.,-1.6));
#21667=CARTESIAN_POINT('Origin',(4.17091003018116,1.,-1.6));
#21668=CARTESIAN_POINT('Origin',(4.17091003018116,1.,-1.6));
#21669=CARTESIAN_POINT('',(3.77091003018116,1.,-1.2));
#21670=CARTESIAN_POINT('Origin',(4.17091003018116,1.,-1.2));
#21671=CARTESIAN_POINT('',(3.77091003018116,1.,-1.6));
#21672=CARTESIAN_POINT('',(3.77091003018116,1.,-1.6));
#21673=CARTESIAN_POINT('Origin',(4.17091003018116,1.,-1.6));
#21674=CARTESIAN_POINT('Origin',(4.17091003018116,1.,-1.2));
#21675=CARTESIAN_POINT('Origin',(4.17091003018116,1.,-1.6));
#21676=CARTESIAN_POINT('',(0.,0.,0.));
#21677=CARTESIAN_POINT('Origin',(9.77091003018116,-1.,-1.6));
#21678=CARTESIAN_POINT('',(9.60591003018116,-1.,-1.2));
#21679=CARTESIAN_POINT('Origin',(9.77091003018116,-1.,-1.2));
#21680=CARTESIAN_POINT('',(9.60591003018116,-1.,-1.6));
#21681=CARTESIAN_POINT('',(9.60591003018116,-1.,-1.6));
#21682=CARTESIAN_POINT('Origin',(9.77091003018116,-1.,-1.6));
#21683=CARTESIAN_POINT('Origin',(9.77091003018116,-1.,-1.6));
#21684=CARTESIAN_POINT('',(9.37091003018116,-1.,-1.2));
#21685=CARTESIAN_POINT('Origin',(9.77091003018116,-1.,-1.2));
#21686=CARTESIAN_POINT('',(9.37091003018116,-1.,-1.6));
#21687=CARTESIAN_POINT('',(9.37091003018116,-1.,-1.6));
#21688=CARTESIAN_POINT('Origin',(9.77091003018116,-1.,-1.6));
#21689=CARTESIAN_POINT('Origin',(9.77091003018116,-1.,-1.2));
#21690=CARTESIAN_POINT('Origin',(9.77091003018116,-1.,-1.6));
#21691=CARTESIAN_POINT('',(0.,0.,0.));
#21692=CARTESIAN_POINT('Origin',(9.77091003018116,1.,-1.6));
#21693=CARTESIAN_POINT('',(9.60591003018116,1.,-1.2));
#21694=CARTESIAN_POINT('Origin',(9.77091003018116,1.,-1.2));
#21695=CARTESIAN_POINT('',(9.60591003018116,1.,-1.6));
#21696=CARTESIAN_POINT('',(9.60591003018116,1.,-1.6));
#21697=CARTESIAN_POINT('Origin',(9.77091003018116,1.,-1.6));
#21698=CARTESIAN_POINT('Origin',(9.77091003018116,1.,-1.6));
#21699=CARTESIAN_POINT('',(9.37091003018116,1.,-1.2));
#21700=CARTESIAN_POINT('Origin',(9.77091003018116,1.,-1.2));
#21701=CARTESIAN_POINT('',(9.37091003018116,1.,-1.6));
#21702=CARTESIAN_POINT('',(9.37091003018116,1.,-1.6));
#21703=CARTESIAN_POINT('Origin',(9.77091003018116,1.,-1.6));
#21704=CARTESIAN_POINT('Origin',(9.77091003018116,1.,-1.2));
#21705=CARTESIAN_POINT('Origin',(9.77091003018116,1.,-1.6));
#21706=CARTESIAN_POINT('',(0.,0.,0.));
#21707=CARTESIAN_POINT('Origin',(6.97091003018116,-0.4,7.));
#21708=CARTESIAN_POINT('',(5.77091003018116,0.4,7.));
#21709=CARTESIAN_POINT('Origin',(6.97091003018116,0.4,7.));
#21710=CARTESIAN_POINT('',(5.77091003018116,-0.4,7.));
#21711=CARTESIAN_POINT('',(5.77091003018116,-0.4,7.));
#21712=CARTESIAN_POINT('Origin',(6.97091003018116,-0.4,7.));
#21713=CARTESIAN_POINT('Origin',(6.97091003018116,-0.4,7.));
#21714=CARTESIAN_POINT('',(5.38091003018116,0.4,7.));
#21715=CARTESIAN_POINT('Origin',(6.97091003018116,0.4,7.));
#21716=CARTESIAN_POINT('',(5.38091003018116,-0.4,7.));
#21717=CARTESIAN_POINT('',(5.38091003018116,-0.4,7.));
#21718=CARTESIAN_POINT('Origin',(6.97091003018116,-0.4,7.));
#21719=CARTESIAN_POINT('Origin',(6.97091003018116,0.4,7.));
#21720=CARTESIAN_POINT('Origin',(6.97091003018116,-0.4,7.));
#21721=CARTESIAN_POINT('',(0.,0.,0.));
#21722=CARTESIAN_POINT('Origin',(5.55669646780806,-2.2,5.58578643762691));
#21723=CARTESIAN_POINT('',(5.49357471024299,-2.1,5.36982198749241));
#21724=CARTESIAN_POINT('',(5.49357471024299,-1.8,5.36982198749241));
#21725=CARTESIAN_POINT('',(5.49357471024299,-2.2,5.36982198749241));
#21726=CARTESIAN_POINT('',(5.34073201767356,-2.1,5.52266468006184));
#21727=CARTESIAN_POINT('Origin',(5.55669646780806,-2.1,5.58578643762691));
#21728=CARTESIAN_POINT('',(5.34073201767356,-1.8,5.52266468006184));
#21729=CARTESIAN_POINT('',(5.34073201767356,-2.2,5.52266468006184));
#21730=CARTESIAN_POINT('Origin',(5.55669646780806,-1.8,5.58578643762691));
#21731=CARTESIAN_POINT('Origin',(5.55669646780806,-2.2,8.4142135623731));
#21732=CARTESIAN_POINT('',(5.34073201767356,-2.1,8.47733531993816));
#21733=CARTESIAN_POINT('',(5.34073201767356,-1.8,8.47733531993816));
#21734=CARTESIAN_POINT('',(5.34073201767356,-2.2,8.47733531993816));
#21735=CARTESIAN_POINT('',(5.493574710243,-2.1,8.6301780125076));
#21736=CARTESIAN_POINT('Origin',(5.55669646780806,-2.1,8.4142135623731));
#21737=CARTESIAN_POINT('',(5.493574710243,-1.8,8.6301780125076));
#21738=CARTESIAN_POINT('',(5.493574710243,-2.2,8.6301780125076));
#21739=CARTESIAN_POINT('Origin',(5.55669646780806,-1.8,8.4142135623731));
#21740=CARTESIAN_POINT('Origin',(8.38512359255425,-2.2,8.4142135623731));
#21741=CARTESIAN_POINT('',(8.44824535011931,-2.1,8.6301780125076));
#21742=CARTESIAN_POINT('',(8.44824535011931,-1.8,8.6301780125076));
#21743=CARTESIAN_POINT('',(8.44824535011932,-2.2,8.6301780125076));
#21744=CARTESIAN_POINT('',(8.60108804268875,-2.1,8.47733531993816));
#21745=CARTESIAN_POINT('Origin',(8.38512359255425,-2.1,8.4142135623731));
#21746=CARTESIAN_POINT('',(8.60108804268875,-1.8,8.47733531993816));
#21747=CARTESIAN_POINT('',(8.60108804268875,-2.2,8.47733531993816));
#21748=CARTESIAN_POINT('Origin',(8.38512359255425,-1.8,8.4142135623731));
#21749=CARTESIAN_POINT('Origin',(8.38512359255425,-2.2,5.58578643762691));
#21750=CARTESIAN_POINT('',(8.60108804268875,-2.1,5.52266468006184));
#21751=CARTESIAN_POINT('',(8.60108804268875,-1.8,5.52266468006184));
#21752=CARTESIAN_POINT('',(8.60108804268875,-2.2,5.52266468006184));
#21753=CARTESIAN_POINT('',(8.44824535011932,-2.1,5.36982198749241));
#21754=CARTESIAN_POINT('Origin',(8.38512359255425,-2.1,5.58578643762691));
#21755=CARTESIAN_POINT('',(8.44824535011932,-1.8,5.36982198749241));
#21756=CARTESIAN_POINT('',(8.44824535011932,-2.2,5.36982198749241));
#21757=CARTESIAN_POINT('Origin',(8.38512359255425,-1.8,5.58578643762691));
#21758=CARTESIAN_POINT('Origin',(6.97091003018116,-2.1,7.));
#21759=CARTESIAN_POINT('Origin',(6.97091003018116,-2.1,7.));
#21760=CARTESIAN_POINT('Origin',(6.97091003018116,-2.1,7.));
#21761=CARTESIAN_POINT('Origin',(6.97091003018116,-2.1,7.));
#21762=CARTESIAN_POINT('Origin',(6.97091003018116,-2.1,7.));
#21763=CARTESIAN_POINT('',(5.77091003018116,-2.1,7.));
#21764=CARTESIAN_POINT('Origin',(6.97091003018116,-2.1,7.));
#21765=CARTESIAN_POINT('Origin',(6.97091003018116,-2.1,7.));
#21766=CARTESIAN_POINT('Origin',(6.97091003018116,-1.8,7.));
#21767=CARTESIAN_POINT('Origin',(6.97091003018116,-2.1,7.));
#21768=CARTESIAN_POINT('Origin',(6.97091003018116,-1.8,7.));
#21769=CARTESIAN_POINT('Origin',(6.97091003018116,-2.1,7.));
#21770=CARTESIAN_POINT('Origin',(6.97091003018116,-1.8,7.));
#21771=CARTESIAN_POINT('Origin',(6.97091003018116,-2.1,7.));
#21772=CARTESIAN_POINT('Origin',(6.97091003018116,-1.8,7.));
#21773=CARTESIAN_POINT('Origin',(6.97091003018116,-1.8,7.));
#21774=CARTESIAN_POINT('',(5.38091003018116,-1.4,7.));
#21775=CARTESIAN_POINT('Origin',(6.97091003018116,-1.4,7.));
#21776=CARTESIAN_POINT('',(5.38091003018116,-1.8,7.));
#21777=CARTESIAN_POINT('',(5.38091003018116,-1.8,7.));
#21778=CARTESIAN_POINT('Origin',(6.97091003018116,-1.8,7.));
#21779=CARTESIAN_POINT('Origin',(6.97091003018116,-1.4,7.));
#21780=CARTESIAN_POINT('',(5.77091003018116,-1.4,7.));
#21781=CARTESIAN_POINT('Origin',(6.97091003018116,-1.4,7.));
#21782=CARTESIAN_POINT('Origin',(6.97091003018116,-2.1,7.));
#21783=CARTESIAN_POINT('',(5.77091003018116,-2.1,7.));
#21784=CARTESIAN_POINT('Origin',(6.97091003018116,-1.8,7.));
#21785=CARTESIAN_POINT('',(0.,0.,0.));
#21786=CARTESIAN_POINT('Origin',(5.55669646780806,1.7,5.58578643762691));
#21787=CARTESIAN_POINT('',(5.66764231833408,1.7,5.22757418455471));
#21788=CARTESIAN_POINT('',(5.66764231833408,2.1,5.22757418455471));
#21789=CARTESIAN_POINT('',(5.66764231833408,1.7,5.22757418455471));
#21790=CARTESIAN_POINT('',(5.19848421473587,1.7,5.69673228815293));
#21791=CARTESIAN_POINT('Origin',(5.55669646780806,1.7,5.58578643762691));
#21792=CARTESIAN_POINT('',(5.19848421473587,2.1,5.69673228815293));
#21793=CARTESIAN_POINT('',(5.19848421473587,1.7,5.69673228815293));
#21794=CARTESIAN_POINT('Origin',(5.55669646780806,2.1,5.58578643762691));
#21795=CARTESIAN_POINT('Origin',(5.55669646780806,1.7,5.58578643762691));
#21796=CARTESIAN_POINT('',(5.49357471024299,1.7,5.36982198749241));
#21797=CARTESIAN_POINT('Origin',(6.97091003018116,1.7,7.));
#21798=CARTESIAN_POINT('',(5.34073201767356,1.7,5.52266468006184));
#21799=CARTESIAN_POINT('Origin',(5.55669646780806,1.7,5.58578643762691));
#21800=CARTESIAN_POINT('Origin',(6.97091003018116,1.7,7.));
#21801=CARTESIAN_POINT('Origin',(5.55669646780806,1.7,8.4142135623731));
#21802=CARTESIAN_POINT('',(5.66764231833408,1.7,8.77242581544529));
#21803=CARTESIAN_POINT('',(5.493574710243,1.7,8.6301780125076));
#21804=CARTESIAN_POINT('Origin',(6.97091003018116,1.7,7.));
#21805=CARTESIAN_POINT('',(5.19848421473587,1.7,8.30326771184707));
#21806=CARTESIAN_POINT('Origin',(5.55669646780806,1.7,8.4142135623731));
#21807=CARTESIAN_POINT('',(5.34073201767356,1.7,8.47733531993816));
#21808=CARTESIAN_POINT('Origin',(6.97091003018116,1.7,7.));
#21809=CARTESIAN_POINT('Origin',(5.55669646780806,1.7,8.4142135623731));
#21810=CARTESIAN_POINT('Origin',(5.55669646780806,1.7,8.4142135623731));
#21811=CARTESIAN_POINT('',(5.66764231833409,2.1,8.77242581544529));
#21812=CARTESIAN_POINT('',(5.66764231833408,1.7,8.77242581544529));
#21813=CARTESIAN_POINT('',(5.19848421473587,2.1,8.30326771184707));
#21814=CARTESIAN_POINT('Origin',(5.55669646780806,2.1,8.4142135623731));
#21815=CARTESIAN_POINT('',(5.19848421473587,1.7,8.30326771184707));
#21816=CARTESIAN_POINT('Origin',(8.38512359255425,1.7,8.4142135623731));
#21817=CARTESIAN_POINT('',(8.74333584562645,1.7,8.30326771184707));
#21818=CARTESIAN_POINT('',(8.60108804268875,1.7,8.47733531993816));
#21819=CARTESIAN_POINT('Origin',(6.97091003018116,1.7,7.));
#21820=CARTESIAN_POINT('',(8.27417774202823,1.7,8.77242581544529));
#21821=CARTESIAN_POINT('Origin',(8.38512359255425,1.7,8.4142135623731));
#21822=CARTESIAN_POINT('',(8.44824535011932,1.7,8.6301780125076));
#21823=CARTESIAN_POINT('Origin',(6.97091003018116,1.7,7.));
#21824=CARTESIAN_POINT('Origin',(8.38512359255425,1.7,8.4142135623731));
#21825=CARTESIAN_POINT('Origin',(8.38512359255425,1.7,8.4142135623731));
#21826=CARTESIAN_POINT('',(8.74333584562645,2.1,8.30326771184707));
#21827=CARTESIAN_POINT('',(8.74333584562645,1.7,8.30326771184707));
#21828=CARTESIAN_POINT('',(8.27417774202823,2.1,8.77242581544529));
#21829=CARTESIAN_POINT('Origin',(8.38512359255425,2.1,8.4142135623731));
#21830=CARTESIAN_POINT('',(8.27417774202823,1.7,8.77242581544529));
#21831=CARTESIAN_POINT('Origin',(8.38512359255425,1.7,5.58578643762691));
#21832=CARTESIAN_POINT('',(8.27417774202823,1.7,5.22757418455471));
#21833=CARTESIAN_POINT('',(8.44824535011932,1.7,5.36982198749241));
#21834=CARTESIAN_POINT('Origin',(6.97091003018116,1.7,7.));
#21835=CARTESIAN_POINT('',(8.74333584562644,1.7,5.69673228815293));
#21836=CARTESIAN_POINT('Origin',(8.38512359255425,1.7,5.58578643762691));
#21837=CARTESIAN_POINT('',(8.60108804268875,1.7,5.52266468006184));
#21838=CARTESIAN_POINT('Origin',(6.97091003018116,1.7,7.));
#21839=CARTESIAN_POINT('Origin',(8.38512359255425,1.7,5.58578643762691));
#21840=CARTESIAN_POINT('Origin',(8.38512359255425,1.7,5.58578643762691));
#21841=CARTESIAN_POINT('',(8.27417774202823,2.1,5.22757418455471));
#21842=CARTESIAN_POINT('',(8.27417774202823,1.7,5.22757418455471));
#21843=CARTESIAN_POINT('',(8.74333584562644,2.1,5.69673228815293));
#21844=CARTESIAN_POINT('Origin',(8.38512359255425,2.1,5.58578643762691));
#21845=CARTESIAN_POINT('',(8.74333584562644,1.7,5.69673228815293));
#21846=CARTESIAN_POINT('Origin',(5.55669646780806,1.7,8.4142135623731));
#21847=CARTESIAN_POINT('',(5.34073201767356,1.4,8.47733531993816));
#21848=CARTESIAN_POINT('',(5.34073201767356,1.7,8.47733531993816));
#21849=CARTESIAN_POINT('',(5.493574710243,1.4,8.6301780125076));
#21850=CARTESIAN_POINT('Origin',(5.55669646780806,1.4,8.4142135623731));
#21851=CARTESIAN_POINT('',(5.493574710243,1.3,8.6301780125076));
#21852=CARTESIAN_POINT('Origin',(8.38512359255425,1.7,8.4142135623731));
#21853=CARTESIAN_POINT('',(8.44824535011931,1.4,8.6301780125076));
#21854=CARTESIAN_POINT('',(8.44824535011932,1.7,8.6301780125076));
#21855=CARTESIAN_POINT('',(8.60108804268875,1.4,8.47733531993816));
#21856=CARTESIAN_POINT('Origin',(8.38512359255425,1.4,8.4142135623731));
#21857=CARTESIAN_POINT('',(8.60108804268875,1.3,8.47733531993816));
#21858=CARTESIAN_POINT('Origin',(8.38512359255425,1.7,5.58578643762691));
#21859=CARTESIAN_POINT('',(8.60108804268875,1.4,5.52266468006184));
#21860=CARTESIAN_POINT('',(8.60108804268875,1.7,5.52266468006184));
#21861=CARTESIAN_POINT('',(8.44824535011932,1.4,5.36982198749241));
#21862=CARTESIAN_POINT('Origin',(8.38512359255425,1.4,5.58578643762691));
#21863=CARTESIAN_POINT('',(8.44824535011932,1.3,5.36982198749241));
#21864=CARTESIAN_POINT('Origin',(6.97091003018116,1.8,7.));
#21865=CARTESIAN_POINT('Origin',(6.97091003018116,2.1,7.));
#21866=CARTESIAN_POINT('',(5.49357471024299,1.4,5.36982198749241));
#21867=CARTESIAN_POINT('Origin',(6.97091003018116,1.4,7.));
#21868=CARTESIAN_POINT('',(5.49357471024299,1.7,5.36982198749241));
#21869=CARTESIAN_POINT('Origin',(6.97091003018116,2.1,7.));
#21870=CARTESIAN_POINT('Origin',(6.97091003018116,2.1,7.));
#21871=CARTESIAN_POINT('Origin',(6.97091003018116,2.1,7.));
#21872=CARTESIAN_POINT('Origin',(6.97091003018116,2.1,7.));
#21873=CARTESIAN_POINT('',(5.77091003018116,2.1,7.));
#21874=CARTESIAN_POINT('Origin',(6.97091003018116,2.1,7.));
#21875=CARTESIAN_POINT('Origin',(6.97091003018116,1.4,7.));
#21876=CARTESIAN_POINT('',(5.34073201767356,1.4,5.52266468006184));
#21877=CARTESIAN_POINT('Origin',(5.55669646780806,1.4,5.58578643762691));
#21878=CARTESIAN_POINT('Origin',(6.97091003018116,1.4,7.));
#21879=CARTESIAN_POINT('Origin',(6.97091003018116,1.4,7.));
#21880=CARTESIAN_POINT('Origin',(6.97091003018116,1.4,7.));
#21881=CARTESIAN_POINT('',(5.77091003018116,1.4,7.));
#21882=CARTESIAN_POINT('Origin',(6.97091003018116,1.4,7.));
#21883=CARTESIAN_POINT('Origin',(6.97091003018116,1.8,7.));
#21884=CARTESIAN_POINT('Origin',(6.97091003018116,1.8,7.));
#21885=CARTESIAN_POINT('Origin',(5.55669646780806,1.7,5.58578643762691));
#21886=CARTESIAN_POINT('',(5.34073201767356,1.3,5.52266468006184));
#21887=CARTESIAN_POINT('Origin',(6.97091003018116,1.8,7.));
#21888=CARTESIAN_POINT('Origin',(6.97091003018116,1.8,7.));
#21889=CARTESIAN_POINT('',(5.77091003018116,1.8,7.));
#21890=CARTESIAN_POINT('',(0.,0.,0.));
#21891=CARTESIAN_POINT('Origin',(6.85463117051588,-3.5,5.73208116779017));
#21892=CARTESIAN_POINT('',(6.85463117051588,-3.425,5.73208116779017));
#21893=CARTESIAN_POINT('',(-0.0581394298326381,-3.425,6.36604058389508));
#21894=CARTESIAN_POINT('',(3.39824587034162,-3.425,6.04906087584262));
#21895=CARTESIAN_POINT('',(6.85463117051588,-2.825,5.73208116779017));
#21896=CARTESIAN_POINT('',(6.85463117051588,-3.5,5.73208116779017));
#21897=CARTESIAN_POINT('',(-0.0581394298326381,-2.825,6.36604058389508));
#21898=CARTESIAN_POINT('',(3.39824587034162,-2.825,6.04906087584262));
#21899=CARTESIAN_POINT('',(-0.0581394298326381,-3.5,6.36604058389508));
#21900=CARTESIAN_POINT('Origin',(-0.0581394298326382,-3.5,7.63395941610492));
#21901=CARTESIAN_POINT('',(-0.0581394298326382,-3.425,7.63395941610492));
#21902=CARTESIAN_POINT('',(6.85463117051588,-3.425,8.26791883220983));
#21903=CARTESIAN_POINT('',(-0.0581394298326382,-3.425,7.63395941610492));
#21904=CARTESIAN_POINT('',(-0.0581394298326382,-2.825,7.63395941610492));
#21905=CARTESIAN_POINT('',(-0.0581394298326382,-3.5,7.63395941610492));
#21906=CARTESIAN_POINT('',(6.85463117051588,-2.825,8.26791883220983));
#21907=CARTESIAN_POINT('',(-0.0581394298326382,-2.825,7.63395941610492));
#21908=CARTESIAN_POINT('',(6.85463117051588,-3.5,8.26791883220983));
#21909=CARTESIAN_POINT('Origin',(0.,-3.425,7.));
#21910=CARTESIAN_POINT('',(-0.067271950114944,-3.425,7.73354152832038));
#21911=CARTESIAN_POINT('',(6.84549865023357,-3.425,8.3675009444253));
#21912=CARTESIAN_POINT('',(-0.067271950114944,-3.425,7.73354152832038));
#21913=CARTESIAN_POINT('',(-0.067271950114944,-3.425,6.26645847167962));
#21914=CARTESIAN_POINT('Origin',(0.,-3.425,7.));
#21915=CARTESIAN_POINT('',(6.84549865023357,-3.425,5.6324990555747));
#21916=CARTESIAN_POINT('',(6.84549865023357,-3.425,5.6324990555747));
#21917=CARTESIAN_POINT('Origin',(6.97091003018116,-3.425,7.));
#21918=CARTESIAN_POINT('Origin',(0.,-3.425,7.));
#21919=CARTESIAN_POINT('Origin',(6.97091003018116,-3.425,7.));
#21920=CARTESIAN_POINT('Origin',(0.,-3.5,7.));
#21921=CARTESIAN_POINT('Origin',(0.,-2.825,7.));
#21922=CARTESIAN_POINT('Origin',(6.97091003018116,-3.5,7.));
#21923=CARTESIAN_POINT('Origin',(6.97091003018116,-2.825,7.));
#21924=CARTESIAN_POINT('Origin',(6.97091003018116,-3.425,7.));
#21925=CARTESIAN_POINT('',(6.84549865023357,-2.825,5.6324990555747));
#21926=CARTESIAN_POINT('',(6.84549865023357,-3.425,5.6324990555747));
#21927=CARTESIAN_POINT('',(6.84549865023357,-2.825,8.3675009444253));
#21928=CARTESIAN_POINT('Origin',(6.97091003018116,-2.825,7.));
#21929=CARTESIAN_POINT('',(6.84549865023357,-3.425,8.3675009444253));
#21930=CARTESIAN_POINT('Origin',(6.84549865023357,-3.425,5.6324990555747));
#21931=CARTESIAN_POINT('',(-0.067271950114944,-2.825,6.26645847167962));
#21932=CARTESIAN_POINT('',(-0.0672719501149439,-3.425,6.26645847167962));
#21933=CARTESIAN_POINT('',(6.84549865023357,-2.825,5.6324990555747));
#21934=CARTESIAN_POINT('Origin',(-0.067271950114944,-3.425,7.73354152832038));
#21935=CARTESIAN_POINT('',(-0.067271950114944,-2.825,7.73354152832038));
#21936=CARTESIAN_POINT('',(-0.067271950114944,-2.825,7.73354152832038));
#21937=CARTESIAN_POINT('',(-0.0672719501149441,-3.425,7.73354152832038));
#21938=CARTESIAN_POINT('Origin',(0.,-3.425,7.));
#21939=CARTESIAN_POINT('Origin',(0.,-2.825,7.));
#21940=CARTESIAN_POINT('Origin',(0.,-2.825,7.));
#21941=CARTESIAN_POINT('',(0.,0.,0.));
#21942=CARTESIAN_POINT('Origin',(12.7709100301812,5.5,1.2));
#21943=CARTESIAN_POINT('',(12.2959100301812,5.5,1.2));
#21944=CARTESIAN_POINT('Origin',(12.7709100301812,5.5,1.2));
#21945=CARTESIAN_POINT('',(12.2959100301812,5.5,3.67));
#21946=CARTESIAN_POINT('',(12.2959100301812,5.5,1.2));
#21947=CARTESIAN_POINT('Origin',(12.7709100301812,5.5,3.67));
#21948=CARTESIAN_POINT('Origin',(12.7709100301812,5.5,1.2));
#21949=CARTESIAN_POINT('',(12.4959100301812,5.5,1.2));
#21950=CARTESIAN_POINT('Origin',(12.7709100301812,5.5,1.2));
#21951=CARTESIAN_POINT('Origin',(12.7709100301812,5.5,-0.1));
#21952=CARTESIAN_POINT('',(12.4959100301812,5.5,0.));
#21953=CARTESIAN_POINT('Origin',(12.7709100301812,5.5,0.));
#21954=CARTESIAN_POINT('',(12.4959100301812,5.5,-0.1));
#21955=CARTESIAN_POINT('Origin',(12.7709100301812,2.5,1.2));
#21956=CARTESIAN_POINT('',(12.2959100301812,2.5,1.2));
#21957=CARTESIAN_POINT('Origin',(12.7709100301812,2.5,1.2));
#21958=CARTESIAN_POINT('',(12.2959100301812,2.5,3.67));
#21959=CARTESIAN_POINT('',(12.2959100301812,2.5,1.2));
#21960=CARTESIAN_POINT('Origin',(12.7709100301812,2.5,3.67));
#21961=CARTESIAN_POINT('Origin',(12.7709100301812,2.5,1.2));
#21962=CARTESIAN_POINT('',(12.4959100301812,2.5,1.2));
#21963=CARTESIAN_POINT('Origin',(12.7709100301812,2.5,1.2));
#21964=CARTESIAN_POINT('Origin',(12.7709100301812,2.5,-0.1));
#21965=CARTESIAN_POINT('',(12.4959100301812,2.5,0.));
#21966=CARTESIAN_POINT('Origin',(12.7709100301812,2.5,0.));
#21967=CARTESIAN_POINT('',(12.4959100301812,2.5,-0.1));
#21968=CARTESIAN_POINT('Origin',(1.17091003018116,5.5,1.2));
#21969=CARTESIAN_POINT('',(0.695910030181156,5.5,1.2));
#21970=CARTESIAN_POINT('Origin',(1.17091003018116,5.5,1.2));
#21971=CARTESIAN_POINT('',(0.695910030181156,5.5,3.67));
#21972=CARTESIAN_POINT('',(0.695910030181156,5.5,1.2));
#21973=CARTESIAN_POINT('Origin',(1.17091003018116,5.5,3.67));
#21974=CARTESIAN_POINT('Origin',(1.17091003018116,5.5,1.2));
#21975=CARTESIAN_POINT('',(0.895910030181156,5.5,1.2));
#21976=CARTESIAN_POINT('Origin',(1.17091003018116,5.5,1.2));
#21977=CARTESIAN_POINT('Origin',(1.17091003018116,5.5,-0.1));
#21978=CARTESIAN_POINT('',(0.895910030181156,5.5,0.));
#21979=CARTESIAN_POINT('Origin',(1.17091003018116,5.5,0.));
#21980=CARTESIAN_POINT('',(0.895910030181156,5.5,-0.1));
#21981=CARTESIAN_POINT('Origin',(1.17091003018116,2.5,1.2));
#21982=CARTESIAN_POINT('',(0.695910030181156,2.5,1.2));
#21983=CARTESIAN_POINT('Origin',(1.17091003018116,2.5,1.2));
#21984=CARTESIAN_POINT('',(0.695910030181156,2.5,3.67));
#21985=CARTESIAN_POINT('',(0.695910030181156,2.5,1.2));
#21986=CARTESIAN_POINT('Origin',(1.17091003018116,2.5,3.67));
#21987=CARTESIAN_POINT('Origin',(1.17091003018116,2.5,1.2));
#21988=CARTESIAN_POINT('',(0.895910030181156,2.5,1.2));
#21989=CARTESIAN_POINT('Origin',(1.17091003018116,2.5,1.2));
#21990=CARTESIAN_POINT('Origin',(1.17091003018116,2.5,-0.1));
#21991=CARTESIAN_POINT('',(0.895910030181156,2.5,0.));
#21992=CARTESIAN_POINT('Origin',(1.17091003018116,2.5,0.));
#21993=CARTESIAN_POINT('',(0.895910030181156,2.5,-0.1));
#21994=CARTESIAN_POINT('Origin',(2.22091003018116,4.,2.));
#21995=CARTESIAN_POINT('',(1.88091003018116,4.,2.));
#21996=CARTESIAN_POINT('Origin',(2.22091003018116,4.,2.));
#21997=CARTESIAN_POINT('',(1.88091003018116,4.,3.67));
#21998=CARTESIAN_POINT('',(1.88091003018116,4.,2.));
#21999=CARTESIAN_POINT('Origin',(2.22091003018116,4.,3.67));
#22000=CARTESIAN_POINT('Origin',(2.22091003018116,4.,2.));
#22001=CARTESIAN_POINT('Origin',(11.7209100301812,4.,2.));
#22002=CARTESIAN_POINT('',(11.3809100301812,4.,2.));
#22003=CARTESIAN_POINT('Origin',(11.7209100301812,4.,2.));
#22004=CARTESIAN_POINT('',(11.3809100301812,4.,3.67));
#22005=CARTESIAN_POINT('',(11.3809100301812,4.,2.));
#22006=CARTESIAN_POINT('Origin',(11.7209100301812,4.,3.67));
#22007=CARTESIAN_POINT('Origin',(11.7209100301812,4.,2.));
#22008=CARTESIAN_POINT('Origin',(13.4709100301812,6.2,0.));
#22009=CARTESIAN_POINT('',(13.4709100301812,6.2,0.));
#22010=CARTESIAN_POINT('',(0.470910030181156,6.2,0.));
#22011=CARTESIAN_POINT('',(13.4709100301812,6.2,0.));
#22012=CARTESIAN_POINT('',(0.470910030181156,6.2,3.67));
#22013=CARTESIAN_POINT('',(0.470910030181156,6.2,0.));
#22014=CARTESIAN_POINT('',(13.4709100301812,6.2,3.67));
#22015=CARTESIAN_POINT('',(13.4709100301812,6.2,3.67));
#22016=CARTESIAN_POINT('',(13.4709100301812,6.2,0.));
#22017=CARTESIAN_POINT('Origin',(13.4709100301812,1.8,0.));
#22018=CARTESIAN_POINT('',(13.4709100301812,1.8,0.));
#22019=CARTESIAN_POINT('',(13.4709100301812,1.8,0.));
#22020=CARTESIAN_POINT('',(13.4709100301812,1.8,3.67));
#22021=CARTESIAN_POINT('',(13.4709100301812,1.8,3.67));
#22022=CARTESIAN_POINT('',(13.4709100301812,1.8,0.));
#22023=CARTESIAN_POINT('Origin',(0.470910030181156,1.8,0.));
#22024=CARTESIAN_POINT('',(0.470910030181156,1.8,0.));
#22025=CARTESIAN_POINT('',(0.470910030181156,1.8,0.));
#22026=CARTESIAN_POINT('',(0.470910030181156,1.8,3.67));
#22027=CARTESIAN_POINT('',(0.470910030181156,1.8,3.67));
#22028=CARTESIAN_POINT('',(0.470910030181156,1.8,0.));
#22029=CARTESIAN_POINT('Origin',(0.470910030181156,6.2,0.));
#22030=CARTESIAN_POINT('',(0.470910030181156,6.2,0.));
#22031=CARTESIAN_POINT('',(0.470910030181156,6.2,3.67));
#22032=CARTESIAN_POINT('Origin',(6.97091003018116,4.,3.67));
#22033=CARTESIAN_POINT('Origin',(6.97091003018116,4.,0.));
#22034=CARTESIAN_POINT('',(0.,0.,0.));
#22035=CARTESIAN_POINT('Origin',(2.22091003018116,4.,3.67));
#22036=CARTESIAN_POINT('',(1.79591003018116,4.,4.87));
#22037=CARTESIAN_POINT('Origin',(2.22091003018116,4.,4.87));
#22038=CARTESIAN_POINT('',(1.79591003018116,4.,3.67));
#22039=CARTESIAN_POINT('',(1.79591003018116,4.,3.67));
#22040=CARTESIAN_POINT('Origin',(2.22091003018116,4.,3.67));
#22041=CARTESIAN_POINT('Origin',(2.22091003018116,4.,3.67));
#22042=CARTESIAN_POINT('',(1.57591003018116,4.,4.87));
#22043=CARTESIAN_POINT('Origin',(2.22091003018116,4.,4.87));
#22044=CARTESIAN_POINT('',(1.57591003018116,4.,3.67));
#22045=CARTESIAN_POINT('',(1.57591003018116,4.,3.67));
#22046=CARTESIAN_POINT('Origin',(2.22091003018116,4.,3.67));
#22047=CARTESIAN_POINT('Origin',(2.22091003018116,4.,4.87));
#22048=CARTESIAN_POINT('Origin',(2.22091003018116,4.,3.67));
#22049=CARTESIAN_POINT('',(0.,0.,0.));
#22050=CARTESIAN_POINT('Origin',(11.7209100301812,4.,3.67));
#22051=CARTESIAN_POINT('',(11.2959100301812,4.,4.87));
#22052=CARTESIAN_POINT('Origin',(11.7209100301812,4.,4.87));
#22053=CARTESIAN_POINT('',(11.2959100301812,4.,3.67));
#22054=CARTESIAN_POINT('',(11.2959100301812,4.,3.67));
#22055=CARTESIAN_POINT('Origin',(11.7209100301812,4.,3.67));
#22056=CARTESIAN_POINT('Origin',(11.7209100301812,4.,3.67));
#22057=CARTESIAN_POINT('',(11.0759100301812,4.,4.87));
#22058=CARTESIAN_POINT('Origin',(11.7209100301812,4.,4.87));
#22059=CARTESIAN_POINT('',(11.0759100301812,4.,3.67));
#22060=CARTESIAN_POINT('',(11.0759100301812,4.,3.67));
#22061=CARTESIAN_POINT('Origin',(11.7209100301812,4.,3.67));
#22062=CARTESIAN_POINT('Origin',(11.7209100301812,4.,4.87));
#22063=CARTESIAN_POINT('Origin',(11.7209100301812,4.,3.67));
#22064=CARTESIAN_POINT('',(0.,0.,0.));
#22065=CARTESIAN_POINT('Origin',(12.7709100301812,41.5,1.2));
#22066=CARTESIAN_POINT('',(12.2959100301812,41.5,1.2));
#22067=CARTESIAN_POINT('Origin',(12.7709100301812,41.5,1.2));
#22068=CARTESIAN_POINT('',(12.2959100301812,41.5,3.67));
#22069=CARTESIAN_POINT('',(12.2959100301812,41.5,1.2));
#22070=CARTESIAN_POINT('Origin',(12.7709100301812,41.5,3.67));
#22071=CARTESIAN_POINT('Origin',(12.7709100301812,41.5,1.2));
#22072=CARTESIAN_POINT('',(12.4959100301812,41.5,1.2));
#22073=CARTESIAN_POINT('Origin',(12.7709100301812,41.5,1.2));
#22074=CARTESIAN_POINT('Origin',(12.7709100301812,41.5,-0.1));
#22075=CARTESIAN_POINT('',(12.4959100301812,41.5,0.));
#22076=CARTESIAN_POINT('Origin',(12.7709100301812,41.5,0.));
#22077=CARTESIAN_POINT('',(12.4959100301812,41.5,-0.1));
#22078=CARTESIAN_POINT('Origin',(12.7709100301812,38.5,1.2));
#22079=CARTESIAN_POINT('',(12.2959100301812,38.5,1.2));
#22080=CARTESIAN_POINT('Origin',(12.7709100301812,38.5,1.2));
#22081=CARTESIAN_POINT('',(12.2959100301812,38.5,3.67));
#22082=CARTESIAN_POINT('',(12.2959100301812,38.5,1.2));
#22083=CARTESIAN_POINT('Origin',(12.7709100301812,38.5,3.67));
#22084=CARTESIAN_POINT('Origin',(12.7709100301812,38.5,1.2));
#22085=CARTESIAN_POINT('',(12.4959100301812,38.5,1.2));
#22086=CARTESIAN_POINT('Origin',(12.7709100301812,38.5,1.2));
#22087=CARTESIAN_POINT('Origin',(12.7709100301812,38.5,-0.1));
#22088=CARTESIAN_POINT('',(12.4959100301812,38.5,0.));
#22089=CARTESIAN_POINT('Origin',(12.7709100301812,38.5,0.));
#22090=CARTESIAN_POINT('',(12.4959100301812,38.5,-0.1));
#22091=CARTESIAN_POINT('Origin',(1.17091003018116,41.5,1.2));
#22092=CARTESIAN_POINT('',(0.695910030181156,41.5,1.2));
#22093=CARTESIAN_POINT('Origin',(1.17091003018116,41.5,1.2));
#22094=CARTESIAN_POINT('',(0.695910030181156,41.5,3.67));
#22095=CARTESIAN_POINT('',(0.695910030181156,41.5,1.2));
#22096=CARTESIAN_POINT('Origin',(1.17091003018116,41.5,3.67));
#22097=CARTESIAN_POINT('Origin',(1.17091003018116,41.5,1.2));
#22098=CARTESIAN_POINT('',(0.895910030181156,41.5,1.2));
#22099=CARTESIAN_POINT('Origin',(1.17091003018116,41.5,1.2));
#22100=CARTESIAN_POINT('Origin',(1.17091003018116,41.5,-0.1));
#22101=CARTESIAN_POINT('',(0.895910030181156,41.5,0.));
#22102=CARTESIAN_POINT('Origin',(1.17091003018116,41.5,0.));
#22103=CARTESIAN_POINT('',(0.895910030181156,41.5,-0.1));
#22104=CARTESIAN_POINT('Origin',(1.17091003018116,38.5,1.2));
#22105=CARTESIAN_POINT('',(0.695910030181156,38.5,1.2));
#22106=CARTESIAN_POINT('Origin',(1.17091003018116,38.5,1.2));
#22107=CARTESIAN_POINT('',(0.695910030181156,38.5,3.67));
#22108=CARTESIAN_POINT('',(0.695910030181156,38.5,1.2));
#22109=CARTESIAN_POINT('Origin',(1.17091003018116,38.5,3.67));
#22110=CARTESIAN_POINT('Origin',(1.17091003018116,38.5,1.2));
#22111=CARTESIAN_POINT('',(0.895910030181156,38.5,1.2));
#22112=CARTESIAN_POINT('Origin',(1.17091003018116,38.5,1.2));
#22113=CARTESIAN_POINT('Origin',(1.17091003018116,38.5,-0.1));
#22114=CARTESIAN_POINT('',(0.895910030181156,38.5,0.));
#22115=CARTESIAN_POINT('Origin',(1.17091003018116,38.5,0.));
#22116=CARTESIAN_POINT('',(0.895910030181156,38.5,-0.1));
#22117=CARTESIAN_POINT('Origin',(2.22091003018116,40.,2.));
#22118=CARTESIAN_POINT('',(1.88091003018116,40.,2.));
#22119=CARTESIAN_POINT('Origin',(2.22091003018116,40.,2.));
#22120=CARTESIAN_POINT('',(1.88091003018116,40.,3.67));
#22121=CARTESIAN_POINT('',(1.88091003018116,40.,2.));
#22122=CARTESIAN_POINT('Origin',(2.22091003018116,40.,3.67));
#22123=CARTESIAN_POINT('Origin',(2.22091003018116,40.,2.));
#22124=CARTESIAN_POINT('Origin',(11.7209100301812,40.,2.));
#22125=CARTESIAN_POINT('',(11.3809100301812,40.,2.));
#22126=CARTESIAN_POINT('Origin',(11.7209100301812,40.,2.));
#22127=CARTESIAN_POINT('',(11.3809100301812,40.,3.67));
#22128=CARTESIAN_POINT('',(11.3809100301812,40.,2.));
#22129=CARTESIAN_POINT('Origin',(11.7209100301812,40.,3.67));
#22130=CARTESIAN_POINT('Origin',(11.7209100301812,40.,2.));
#22131=CARTESIAN_POINT('Origin',(13.4709100301812,42.2,0.));
#22132=CARTESIAN_POINT('',(13.4709100301812,42.2,0.));
#22133=CARTESIAN_POINT('',(0.470910030181156,42.2,0.));
#22134=CARTESIAN_POINT('',(13.4709100301812,42.2,0.));
#22135=CARTESIAN_POINT('',(0.470910030181156,42.2,3.67));
#22136=CARTESIAN_POINT('',(0.470910030181156,42.2,0.));
#22137=CARTESIAN_POINT('',(13.4709100301812,42.2,3.67));
#22138=CARTESIAN_POINT('',(13.4709100301812,42.2,3.67));
#22139=CARTESIAN_POINT('',(13.4709100301812,42.2,0.));
#22140=CARTESIAN_POINT('Origin',(13.4709100301812,37.8,0.));
#22141=CARTESIAN_POINT('',(13.4709100301812,37.8,0.));
#22142=CARTESIAN_POINT('',(13.4709100301812,37.8,0.));
#22143=CARTESIAN_POINT('',(13.4709100301812,37.8,3.67));
#22144=CARTESIAN_POINT('',(13.4709100301812,37.8,3.67));
#22145=CARTESIAN_POINT('',(13.4709100301812,37.8,0.));
#22146=CARTESIAN_POINT('Origin',(0.470910030181156,37.8,0.));
#22147=CARTESIAN_POINT('',(0.470910030181156,37.8,0.));
#22148=CARTESIAN_POINT('',(0.470910030181156,37.8,0.));
#22149=CARTESIAN_POINT('',(0.470910030181156,37.8,3.67));
#22150=CARTESIAN_POINT('',(0.470910030181156,37.8,3.67));
#22151=CARTESIAN_POINT('',(0.470910030181156,37.8,0.));
#22152=CARTESIAN_POINT('Origin',(0.470910030181156,42.2,0.));
#22153=CARTESIAN_POINT('',(0.470910030181156,42.2,0.));
#22154=CARTESIAN_POINT('',(0.470910030181156,42.2,3.67));
#22155=CARTESIAN_POINT('Origin',(6.97091003018116,40.,3.67));
#22156=CARTESIAN_POINT('Origin',(6.97091003018116,40.,0.));
#22157=CARTESIAN_POINT('',(0.,0.,0.));
#22158=CARTESIAN_POINT('Origin',(2.22091003018116,40.,3.67));
#22159=CARTESIAN_POINT('',(1.79591003018116,40.,4.87));
#22160=CARTESIAN_POINT('Origin',(2.22091003018116,40.,4.87));
#22161=CARTESIAN_POINT('',(1.79591003018116,40.,3.67));
#22162=CARTESIAN_POINT('',(1.79591003018116,40.,3.67));
#22163=CARTESIAN_POINT('Origin',(2.22091003018116,40.,3.67));
#22164=CARTESIAN_POINT('Origin',(2.22091003018116,40.,3.67));
#22165=CARTESIAN_POINT('',(1.57591003018116,40.,4.87));
#22166=CARTESIAN_POINT('Origin',(2.22091003018116,40.,4.87));
#22167=CARTESIAN_POINT('',(1.57591003018116,40.,3.67));
#22168=CARTESIAN_POINT('',(1.57591003018116,40.,3.67));
#22169=CARTESIAN_POINT('Origin',(2.22091003018116,40.,3.67));
#22170=CARTESIAN_POINT('Origin',(2.22091003018116,40.,4.87));
#22171=CARTESIAN_POINT('Origin',(2.22091003018116,40.,3.67));
#22172=CARTESIAN_POINT('',(0.,0.,0.));
#22173=CARTESIAN_POINT('Origin',(11.7209100301812,40.,3.67));
#22174=CARTESIAN_POINT('',(11.2959100301812,40.,4.87));
#22175=CARTESIAN_POINT('Origin',(11.7209100301812,40.,4.87));
#22176=CARTESIAN_POINT('',(11.2959100301812,40.,3.67));
#22177=CARTESIAN_POINT('',(11.2959100301812,40.,3.67));
#22178=CARTESIAN_POINT('Origin',(11.7209100301812,40.,3.67));
#22179=CARTESIAN_POINT('Origin',(11.7209100301812,40.,3.67));
#22180=CARTESIAN_POINT('',(11.0759100301812,40.,4.87));
#22181=CARTESIAN_POINT('Origin',(11.7209100301812,40.,4.87));
#22182=CARTESIAN_POINT('',(11.0759100301812,40.,3.67));
#22183=CARTESIAN_POINT('',(11.0759100301812,40.,3.67));
#22184=CARTESIAN_POINT('Origin',(11.7209100301812,40.,3.67));
#22185=CARTESIAN_POINT('Origin',(11.7209100301812,40.,4.87));
#22186=CARTESIAN_POINT('Origin',(11.7209100301812,40.,3.67));
#22187=CARTESIAN_POINT('',(0.,0.,0.));
#22188=CARTESIAN_POINT('Origin',(-1.5,8.5,0.8));
#22189=CARTESIAN_POINT('',(-1.9,8.5,0.8));
#22190=CARTESIAN_POINT('Origin',(-1.5,8.5,0.8));
#22191=CARTESIAN_POINT('',(-1.9,8.5,4.9));
#22192=CARTESIAN_POINT('',(-1.9,8.5,0.8));
#22193=CARTESIAN_POINT('Origin',(-1.5,8.5,4.9));
#22194=CARTESIAN_POINT('Origin',(-1.5,8.5,0.8));
#22195=CARTESIAN_POINT('',(-1.725,8.5,0.8));
#22196=CARTESIAN_POINT('Origin',(-1.5,8.5,0.8));
#22197=CARTESIAN_POINT('Origin',(-1.5,8.5,-0.1));
#22198=CARTESIAN_POINT('',(-1.725,8.5,0.));
#22199=CARTESIAN_POINT('Origin',(-1.5,8.5,0.));
#22200=CARTESIAN_POINT('',(-1.725,8.5,-0.1));
#22201=CARTESIAN_POINT('Origin',(-1.5,4.5,0.8));
#22202=CARTESIAN_POINT('',(-1.9,4.5,0.8));
#22203=CARTESIAN_POINT('Origin',(-1.5,4.5,0.8));
#22204=CARTESIAN_POINT('',(-1.9,4.5,4.9));
#22205=CARTESIAN_POINT('',(-1.9,4.5,0.8));
#22206=CARTESIAN_POINT('Origin',(-1.5,4.5,4.9));
#22207=CARTESIAN_POINT('Origin',(-1.5,4.5,0.8));
#22208=CARTESIAN_POINT('',(-1.725,4.5,0.8));
#22209=CARTESIAN_POINT('Origin',(-1.5,4.5,0.8));
#22210=CARTESIAN_POINT('Origin',(-1.5,4.5,-0.1));
#22211=CARTESIAN_POINT('',(-1.725,4.5,0.));
#22212=CARTESIAN_POINT('Origin',(-1.5,4.5,0.));
#22213=CARTESIAN_POINT('',(-1.725,4.5,-0.1));
#22214=CARTESIAN_POINT('Origin',(0.,9.,0.));
#22215=CARTESIAN_POINT('',(0.,9.,0.));
#22216=CARTESIAN_POINT('',(-2.5,9.,0.));
#22217=CARTESIAN_POINT('',(0.,9.,0.));
#22218=CARTESIAN_POINT('',(-2.5,9.,4.9));
#22219=CARTESIAN_POINT('',(-2.5,9.,0.));
#22220=CARTESIAN_POINT('',(0.,9.,4.9));
#22221=CARTESIAN_POINT('',(0.,9.,4.9));
#22222=CARTESIAN_POINT('',(0.,9.,0.));
#22223=CARTESIAN_POINT('Origin',(0.,4.,0.));
#22224=CARTESIAN_POINT('',(0.,4.,0.));
#22225=CARTESIAN_POINT('',(0.,4.,0.));
#22226=CARTESIAN_POINT('',(0.,4.,4.9));
#22227=CARTESIAN_POINT('',(0.,4.,4.9));
#22228=CARTESIAN_POINT('',(0.,4.,0.));
#22229=CARTESIAN_POINT('Origin',(-2.5,4.,0.));
#22230=CARTESIAN_POINT('',(-2.5,4.,0.));
#22231=CARTESIAN_POINT('',(-2.5,4.,0.));
#22232=CARTESIAN_POINT('',(-2.5,4.,4.9));
#22233=CARTESIAN_POINT('',(-2.5,4.,4.9));
#22234=CARTESIAN_POINT('',(-2.5,4.,0.));
#22235=CARTESIAN_POINT('Origin',(-2.5,9.,0.));
#22236=CARTESIAN_POINT('',(-2.5,9.,0.));
#22237=CARTESIAN_POINT('',(-2.5,9.,4.9));
#22238=CARTESIAN_POINT('Origin',(-1.25,6.5,4.9));
#22239=CARTESIAN_POINT('Origin',(-1.25,6.5,0.));
#22240=CARTESIAN_POINT('',(0.,0.,0.));
#22241=CARTESIAN_POINT('Origin',(2.1,10.,4.9));
#22242=CARTESIAN_POINT('',(2.1,10.,4.9));
#22243=CARTESIAN_POINT('',(-2.1,10.,4.9));
#22244=CARTESIAN_POINT('',(2.1,10.,4.9));
#22245=CARTESIAN_POINT('',(-2.1,10.,9.1));
#22246=CARTESIAN_POINT('',(-2.1,10.,4.9));
#22247=CARTESIAN_POINT('',(2.1,10.,9.1));
#22248=CARTESIAN_POINT('',(2.1,10.,9.1));
#22249=CARTESIAN_POINT('',(2.1,10.,4.9));
#22250=CARTESIAN_POINT('Origin',(2.1,5.,4.9));
#22251=CARTESIAN_POINT('',(2.1,5.,4.9));
#22252=CARTESIAN_POINT('',(2.1,5.,4.9));
#22253=CARTESIAN_POINT('',(2.1,5.,9.1));
#22254=CARTESIAN_POINT('',(2.1,5.,9.1));
#22255=CARTESIAN_POINT('',(2.1,5.,4.9));
#22256=CARTESIAN_POINT('Origin',(-2.1,5.,4.9));
#22257=CARTESIAN_POINT('',(-2.1,5.,4.9));
#22258=CARTESIAN_POINT('',(-2.1,5.,4.9));
#22259=CARTESIAN_POINT('',(-2.1,5.,9.1));
#22260=CARTESIAN_POINT('',(-2.1,5.,9.1));
#22261=CARTESIAN_POINT('',(-2.1,5.,4.9));
#22262=CARTESIAN_POINT('Origin',(-2.1,10.,4.9));
#22263=CARTESIAN_POINT('',(-2.1,10.,4.9));
#22264=CARTESIAN_POINT('',(-2.1,10.,9.1));
#22265=CARTESIAN_POINT('Origin',(0.,7.5,9.1));
#22266=CARTESIAN_POINT('Origin',(0.,7.5,4.9));
#22267=CARTESIAN_POINT('',(0.,0.,0.));
#22268=CARTESIAN_POINT('Origin',(-3.,-6.1,4.5));
#22269=CARTESIAN_POINT('',(-3.165,-6.,4.5));
#22270=CARTESIAN_POINT('Origin',(-3.,-6.,4.5));
#22271=CARTESIAN_POINT('',(-3.165,-5.,4.5));
#22272=CARTESIAN_POINT('',(-3.165,-6.1,4.5));
#22273=CARTESIAN_POINT('Origin',(-3.,-5.,4.5));
#22274=CARTESIAN_POINT('Origin',(-3.,-6.1,10.));
#22275=CARTESIAN_POINT('',(-3.165,-6.,10.));
#22276=CARTESIAN_POINT('Origin',(-3.,-6.,10.));
#22277=CARTESIAN_POINT('',(-3.165,-5.,10.));
#22278=CARTESIAN_POINT('',(-3.165,-6.1,10.));
#22279=CARTESIAN_POINT('Origin',(-3.,-5.,10.));
#22280=CARTESIAN_POINT('Origin',(-2.6,-5.,0.));
#22281=CARTESIAN_POINT('',(-2.6,-5.,0.));
#22282=CARTESIAN_POINT('',(-3.4,-5.,0.));
#22283=CARTESIAN_POINT('',(-2.6,-5.,0.));
#22284=CARTESIAN_POINT('',(-3.4,-5.,11.));
#22285=CARTESIAN_POINT('',(-3.4,-5.,0.));
#22286=CARTESIAN_POINT('',(-2.6,-5.,11.));
#22287=CARTESIAN_POINT('',(-2.6,-5.,11.));
#22288=CARTESIAN_POINT('',(-2.6,-5.,0.));
#22289=CARTESIAN_POINT('Origin',(-2.6,-6.,0.));
#22290=CARTESIAN_POINT('',(-2.6,-6.,0.));
#22291=CARTESIAN_POINT('',(-2.6,-6.,0.));
#22292=CARTESIAN_POINT('',(-2.6,-6.,11.));
#22293=CARTESIAN_POINT('',(-2.6,-6.,11.));
#22294=CARTESIAN_POINT('',(-2.6,-6.,0.));
#22295=CARTESIAN_POINT('Origin',(-3.4,-6.,0.));
#22296=CARTESIAN_POINT('',(-3.4,-6.,0.));
#22297=CARTESIAN_POINT('',(-3.4,-6.,0.));
#22298=CARTESIAN_POINT('',(-3.4,-6.,11.));
#22299=CARTESIAN_POINT('',(-3.4,-6.,11.));
#22300=CARTESIAN_POINT('',(-3.4,-6.,0.));
#22301=CARTESIAN_POINT('Origin',(-3.4,-5.,0.));
#22302=CARTESIAN_POINT('',(-3.4,-5.,0.));
#22303=CARTESIAN_POINT('',(-3.4,-5.,11.));
#22304=CARTESIAN_POINT('Origin',(-3.,-5.5,11.));
#22305=CARTESIAN_POINT('Origin',(-3.,-5.5,0.));
#22306=CARTESIAN_POINT('',(0.,0.,0.));
#22307=CARTESIAN_POINT('Origin',(9.97091003018116,-6.1,4.5));
#22308=CARTESIAN_POINT('',(9.80591003018116,-6.,4.5));
#22309=CARTESIAN_POINT('Origin',(9.97091003018116,-6.,4.5));
#22310=CARTESIAN_POINT('',(9.80591003018116,-5.,4.5));
#22311=CARTESIAN_POINT('',(9.80591003018116,-6.1,4.5));
#22312=CARTESIAN_POINT('Origin',(9.97091003018116,-5.,4.5));
#22313=CARTESIAN_POINT('Origin',(9.97091003018116,-6.1,10.));
#22314=CARTESIAN_POINT('',(9.80591003018116,-6.,10.));
#22315=CARTESIAN_POINT('Origin',(9.97091003018116,-6.,10.));
#22316=CARTESIAN_POINT('',(9.80591003018116,-5.,10.));
#22317=CARTESIAN_POINT('',(9.80591003018116,-6.1,10.));
#22318=CARTESIAN_POINT('Origin',(9.97091003018116,-5.,10.));
#22319=CARTESIAN_POINT('Origin',(10.3709100301812,-5.,0.));
#22320=CARTESIAN_POINT('',(10.3709100301812,-5.,0.));
#22321=CARTESIAN_POINT('',(9.57091003018116,-5.,0.));
#22322=CARTESIAN_POINT('',(10.3709100301812,-5.,0.));
#22323=CARTESIAN_POINT('',(9.57091003018116,-5.,11.));
#22324=CARTESIAN_POINT('',(9.57091003018116,-5.,0.));
#22325=CARTESIAN_POINT('',(10.3709100301812,-5.,11.));
#22326=CARTESIAN_POINT('',(10.3709100301812,-5.,11.));
#22327=CARTESIAN_POINT('',(10.3709100301812,-5.,0.));
#22328=CARTESIAN_POINT('Origin',(10.3709100301812,-6.,0.));
#22329=CARTESIAN_POINT('',(10.3709100301812,-6.,0.));
#22330=CARTESIAN_POINT('',(10.3709100301812,-6.,0.));
#22331=CARTESIAN_POINT('',(10.3709100301812,-6.,11.));
#22332=CARTESIAN_POINT('',(10.3709100301812,-6.,11.));
#22333=CARTESIAN_POINT('',(10.3709100301812,-6.,0.));
#22334=CARTESIAN_POINT('Origin',(9.57091003018116,-6.,0.));
#22335=CARTESIAN_POINT('',(9.57091003018116,-6.,0.));
#22336=CARTESIAN_POINT('',(9.57091003018116,-6.,0.));
#22337=CARTESIAN_POINT('',(9.57091003018116,-6.,11.));
#22338=CARTESIAN_POINT('',(9.57091003018116,-6.,11.));
#22339=CARTESIAN_POINT('',(9.57091003018116,-6.,0.));
#22340=CARTESIAN_POINT('Origin',(9.57091003018116,-5.,0.));
#22341=CARTESIAN_POINT('',(9.57091003018116,-5.,0.));
#22342=CARTESIAN_POINT('',(9.57091003018116,-5.,11.));
#22343=CARTESIAN_POINT('Origin',(9.97091003018116,-5.5,11.));
#22344=CARTESIAN_POINT('Origin',(9.97091003018116,-5.5,0.));
#22345=CARTESIAN_POINT('',(0.,0.,0.));
#22346=CARTESIAN_POINT('Origin',(9.97091003018116,-6.3,4.5));
#22347=CARTESIAN_POINT('',(9.74591003018116,-6.2,4.5));
#22348=CARTESIAN_POINT('Origin',(9.97091003018116,-6.2,4.5));
#22349=CARTESIAN_POINT('',(9.74591003018116,-6.,4.5));
#22350=CARTESIAN_POINT('',(9.74591003018116,-6.3,4.5));
#22351=CARTESIAN_POINT('Origin',(9.97091003018116,-6.,4.5));
#22352=CARTESIAN_POINT('Origin',(-3.,-6.3,10.));
#22353=CARTESIAN_POINT('',(-3.225,-6.2,10.));
#22354=CARTESIAN_POINT('Origin',(-3.,-6.2,10.));
#22355=CARTESIAN_POINT('',(-3.225,-6.,10.));
#22356=CARTESIAN_POINT('',(-3.225,-6.3,10.));
#22357=CARTESIAN_POINT('Origin',(-3.,-6.,10.));
#22358=CARTESIAN_POINT('Origin',(-3.,-6.3,4.5));
#22359=CARTESIAN_POINT('',(-3.225,-6.2,4.5));
#22360=CARTESIAN_POINT('Origin',(-3.,-6.2,4.5));
#22361=CARTESIAN_POINT('',(-3.225,-6.,4.5));
#22362=CARTESIAN_POINT('',(-3.225,-6.3,4.5));
#22363=CARTESIAN_POINT('Origin',(-3.,-6.,4.5));
#22364=CARTESIAN_POINT('Origin',(9.97091003018116,-6.3,10.));
#22365=CARTESIAN_POINT('',(9.74591003018116,-6.2,10.));
#22366=CARTESIAN_POINT('Origin',(9.97091003018116,-6.2,10.));
#22367=CARTESIAN_POINT('',(9.74591003018116,-6.,10.));
#22368=CARTESIAN_POINT('',(9.74591003018116,-6.3,10.));
#22369=CARTESIAN_POINT('Origin',(9.97091003018116,-6.,10.));
#22370=CARTESIAN_POINT('Origin',(-3.4,-6.2,3.5));
#22371=CARTESIAN_POINT('',(-3.4,-6.2,11.));
#22372=CARTESIAN_POINT('',(-3.4,-6.2,3.5));
#22373=CARTESIAN_POINT('',(-3.4,-6.2,11.));
#22374=CARTESIAN_POINT('',(-3.4,-6.,11.));
#22375=CARTESIAN_POINT('',(-3.4,-6.2,11.));
#22376=CARTESIAN_POINT('',(-3.4,-6.,3.5));
#22377=CARTESIAN_POINT('',(-3.4,-6.,11.));
#22378=CARTESIAN_POINT('',(-3.4,-6.2,3.5));
#22379=CARTESIAN_POINT('Origin',(10.3709100301812,-6.2,3.5));
#22380=CARTESIAN_POINT('',(10.3709100301812,-6.2,3.5));
#22381=CARTESIAN_POINT('',(-3.4,-6.2,3.5));
#22382=CARTESIAN_POINT('',(10.3709100301812,-6.,3.5));
#22383=CARTESIAN_POINT('',(-3.4,-6.,3.5));
#22384=CARTESIAN_POINT('',(10.3709100301812,-6.2,3.5));
#22385=CARTESIAN_POINT('Origin',(10.3709100301812,-6.2,11.));
#22386=CARTESIAN_POINT('',(10.3709100301812,-6.2,11.));
#22387=CARTESIAN_POINT('',(10.3709100301812,-6.2,3.5));
#22388=CARTESIAN_POINT('',(10.3709100301812,-6.,11.));
#22389=CARTESIAN_POINT('',(10.3709100301812,-6.,3.5));
#22390=CARTESIAN_POINT('',(10.3709100301812,-6.2,11.));
#22391=CARTESIAN_POINT('Origin',(-3.4,-6.2,11.));
#22392=CARTESIAN_POINT('',(10.3709100301812,-6.2,11.));
#22393=CARTESIAN_POINT('',(10.3709100301812,-6.,11.));
#22394=CARTESIAN_POINT('Origin',(3.48545501509058,-6.,7.25));
#22395=CARTESIAN_POINT('Origin',(3.48545501509058,-6.2,7.25));
#22396=CARTESIAN_POINT('',(0.,0.,0.));
#22397=CARTESIAN_POINT('',(0.,0.,0.));
#22398=CARTESIAN_POINT('Origin',(0.,0.,0.));
#22399=CARTESIAN_POINT('',(-0.976185,-0.246528389340863,-1.19548183562566E-16));
#22400=CARTESIAN_POINT('',(-1.19548183562566E-16,-0.246528389340863,0.976185));
#22401=CARTESIAN_POINT('Origin',(0.,-0.246528389340863,0.));
#22402=CARTESIAN_POINT('Origin',(0.,-0.246528389340863,0.));
#22403=CARTESIAN_POINT('',(-1.19548183562566E-16,0.246528389340863,0.976185));
#22404=CARTESIAN_POINT('Origin',(-1.22464679914735E-16,0.,1.));
#22405=CARTESIAN_POINT('',(-0.976185,0.246528389340863,1.19548183562566E-16));
#22406=CARTESIAN_POINT('Origin',(0.,0.246528389340863,0.));
#22407=CARTESIAN_POINT('Origin',(0.,0.246528389340863,0.));
#22408=CARTESIAN_POINT('Origin',(0.,0.,0.));
#22409=CARTESIAN_POINT('',(-0.976185,0.45,-1.19548183562566E-16));
#22410=CARTESIAN_POINT('',(-0.976185,0.,-1.19548183562566E-16));
#22411=CARTESIAN_POINT('Origin',(0.,0.45,0.));
#22412=CARTESIAN_POINT('Origin',(0.,0.,0.));
#22413=CARTESIAN_POINT('',(-0.5,-0.39,-6.12323399573677E-17));
#22414=CARTESIAN_POINT('Origin',(0.,-0.39,0.));
#22415=CARTESIAN_POINT('',(-0.5,0.39,-6.12323399573677E-17));
#22416=CARTESIAN_POINT('',(-0.5,0.,-6.12323399573677E-17));
#22417=CARTESIAN_POINT('Origin',(0.,0.39,0.));
#22418=CARTESIAN_POINT('Origin',(0.,0.42,0.));
#22419=CARTESIAN_POINT('',(-0.56,0.45,-6.85802207522518E-17));
#22420=CARTESIAN_POINT('',(-0.53,0.42,-6.49062803548097E-17));
#22421=CARTESIAN_POINT('Origin',(0.,0.45,0.));
#22422=CARTESIAN_POINT('Origin',(0.976185,0.45,0.));
#22423=CARTESIAN_POINT('Origin',(0.,0.,0.));
#22424=CARTESIAN_POINT('',(-0.976185,-0.45,-1.19548183562566E-16));
#22425=CARTESIAN_POINT('Origin',(0.,-0.45,0.));
#22426=CARTESIAN_POINT('',(-0.976185,0.,-1.19548183562566E-16));
#22427=CARTESIAN_POINT('Origin',(0.56,-0.45,0.));
#22428=CARTESIAN_POINT('',(-0.56,-0.45,-6.85802207522518E-17));
#22429=CARTESIAN_POINT('Origin',(0.,-0.45,0.));
#22430=CARTESIAN_POINT('Origin',(0.,-0.42,0.));
#22431=CARTESIAN_POINT('',(-0.53,-0.42,-6.49062803548097E-17));
#22432=CARTESIAN_POINT('',(0.,0.,0.));
#22433=CARTESIAN_POINT('Origin',(0.,0.,0.));
#22434=CARTESIAN_POINT('',(-1.023815,0.246528389340863,-1.25381176266905E-16));
#22435=CARTESIAN_POINT('',(-1.25381176266905E-16,0.246528389340863,1.023815));
#22436=CARTESIAN_POINT('Origin',(0.,0.246528389340863,0.));
#22437=CARTESIAN_POINT('Origin',(0.,0.246528389340863,0.));
#22438=CARTESIAN_POINT('',(-1.25381176266905E-16,-0.246528389340863,1.023815));
#22439=CARTESIAN_POINT('Origin',(-1.22464679914735E-16,0.,1.));
#22440=CARTESIAN_POINT('',(-1.023815,-0.246528389340863,1.25381176266905E-16));
#22441=CARTESIAN_POINT('Origin',(0.,-0.246528389340863,0.));
#22442=CARTESIAN_POINT('Origin',(0.,-0.246528389340863,0.));
#22443=CARTESIAN_POINT('Origin',(0.,0.,0.));
#22444=CARTESIAN_POINT('',(-1.023815,-0.45,-1.25381176266905E-16));
#22445=CARTESIAN_POINT('Origin',(0.,-0.45,0.));
#22446=CARTESIAN_POINT('',(-1.023815,0.,-1.25381176266905E-16));
#22447=CARTESIAN_POINT('Origin',(1.44,0.45,0.));
#22448=CARTESIAN_POINT('',(-1.44,0.45,-1.76349139077219E-16));
#22449=CARTESIAN_POINT('Origin',(0.,0.45,0.));
#22450=CARTESIAN_POINT('',(-1.023815,0.45,-1.25381176266905E-16));
#22451=CARTESIAN_POINT('Origin',(0.,0.45,0.));
#22452=CARTESIAN_POINT('Origin',(0.,0.42,0.));
#22453=CARTESIAN_POINT('',(-1.5,0.39,-1.83697019872103E-16));
#22454=CARTESIAN_POINT('Origin',(0.,0.39,0.));
#22455=CARTESIAN_POINT('',(-1.47,0.42,-1.80023079474661E-16));
#22456=CARTESIAN_POINT('Origin',(0.,0.,0.));
#22457=CARTESIAN_POINT('',(-1.5,-0.39,-1.83697019872103E-16));
#22458=CARTESIAN_POINT('Origin',(0.,-0.39,0.));
#22459=CARTESIAN_POINT('',(-1.5,0.,-1.83697019872103E-16));
#22460=CARTESIAN_POINT('Origin',(0.,-0.42,0.));
#22461=CARTESIAN_POINT('',(-1.44,-0.45,-1.76349139077219E-16));
#22462=CARTESIAN_POINT('Origin',(0.,-0.45,0.));
#22463=CARTESIAN_POINT('',(-1.47,-0.42,-1.80023079474661E-16));
#22464=CARTESIAN_POINT('Origin',(1.023815,-0.45,0.));
#22465=CARTESIAN_POINT('Origin',(0.,0.,0.));
#22466=CARTESIAN_POINT('',(-1.023815,0.,-1.25381176266905E-16));
#22467=CARTESIAN_POINT('',(0.,0.,0.));
#22468=CARTESIAN_POINT('Origin',(1.,0.,0.));
#22469=CARTESIAN_POINT('',(1.,-1.78583896120461E-33,0.23815));
#22470=CARTESIAN_POINT('',(1.,-1.78583896120461E-33,-0.23815));
#22471=CARTESIAN_POINT('Origin',(1.,0.,0.));
#22472=CARTESIAN_POINT('Origin',(0.707106781186548,0.,-0.707106781186547));
#22473=CARTESIAN_POINT('',(0.875504261126124,-1.78583896120461E-33,-0.538709301246971));
#22474=CARTESIAN_POINT('',(0.538709301246971,-1.78583896120461E-33,-0.875504261126124));
#22475=CARTESIAN_POINT('Origin',(0.707106781186548,0.,-0.707106781186547));
#22476=CARTESIAN_POINT('Origin',(6.12323399573677E-17,0.,-1.));
#22477=CARTESIAN_POINT('',(0.23815,-1.78583896120461E-33,-1.));
#22478=CARTESIAN_POINT('',(-0.23815,-1.78583896120461E-33,-1.));
#22479=CARTESIAN_POINT('Origin',(6.12323399573677E-17,0.,-1.));
#22480=CARTESIAN_POINT('Origin',(-0.707106781186547,0.,-0.707106781186548));
#22481=CARTESIAN_POINT('',(-0.538709301246971,-1.78583896120461E-33,-0.875504261126124));
#22482=CARTESIAN_POINT('',(-0.875504261126124,-1.78583896120461E-33,-0.538709301246971));
#22483=CARTESIAN_POINT('Origin',(-0.707106781186547,0.,-0.707106781186548));
#22484=CARTESIAN_POINT('Origin',(-1.,0.,-1.22464679914735E-16));
#22485=CARTESIAN_POINT('',(-1.,-1.78583896120461E-33,-0.23815));
#22486=CARTESIAN_POINT('',(-1.,-1.78583896120461E-33,0.23815));
#22487=CARTESIAN_POINT('Origin',(-1.,0.,-1.22464679914735E-16));
#22488=CARTESIAN_POINT('Origin',(-0.707106781186548,0.,0.707106781186547));
#22489=CARTESIAN_POINT('',(-0.875504261126124,-7.94881478324376E-33,0.538709301246971));
#22490=CARTESIAN_POINT('',(-0.538709301246971,4.37713686083455E-33,0.875504261126124));
#22491=CARTESIAN_POINT('Origin',(-0.707106781186548,0.,0.707106781186547));
#22492=CARTESIAN_POINT('Origin',(-1.83697019872103E-16,0.,1.));
#22493=CARTESIAN_POINT('',(-0.23815,-1.78583896120461E-33,1.));
#22494=CARTESIAN_POINT('',(0.23815,-1.78583896120461E-33,1.));
#22495=CARTESIAN_POINT('Origin',(-1.83697019872103E-16,0.,1.));
#22496=CARTESIAN_POINT('Origin',(0.707106781186547,0.,0.707106781186548));
#22497=CARTESIAN_POINT('',(0.538709301246971,-4.86732687222419E-33,0.875504261126124));
#22498=CARTESIAN_POINT('',(0.875504261126124,1.29564894981497E-33,0.538709301246971));
#22499=CARTESIAN_POINT('Origin',(0.707106781186547,0.,0.707106781186548));
#22500=CARTESIAN_POINT('',(0.,0.,0.));
#22501=CARTESIAN_POINT('Origin',(0.707106781186547,0.,0.707106781186548));
#22502=CARTESIAN_POINT('',(0.504455939115715,-0.04763,0.841298510752802));
#22503=CARTESIAN_POINT('',(0.841298510752802,-0.04763,0.504455939115715));
#22504=CARTESIAN_POINT('Ctrl Pts',(0.504455939115715,-0.04763,0.841298510752802));
#22505=CARTESIAN_POINT('Ctrl Pts',(0.508899795931835,-0.0740444353928835,
0.838633903678357));
#22506=CARTESIAN_POINT('Ctrl Pts',(0.517157748491652,-0.0999305678883309,
0.833661031856294));
#22507=CARTESIAN_POINT('Ctrl Pts',(0.537715343527944,-0.142345102874864,
0.820511285096538));
#22508=CARTESIAN_POINT('Ctrl Pts',(0.548874290046456,-0.159766064500479,
0.813159949759));
#22509=CARTESIAN_POINT('Ctrl Pts',(0.573915184558107,-0.190326085855194,
0.795684265985089));
#22510=CARTESIAN_POINT('Ctrl Pts',(0.587792702767295,-0.203463743702801,
0.78555112003688));
#22511=CARTESIAN_POINT('Ctrl Pts',(0.615966552324775,-0.224161999508995,
0.763642258217233));
#22512=CARTESIAN_POINT('Ctrl Pts',(0.631684198665438,-0.232861760990032,
0.750785745543687));
#22513=CARTESIAN_POINT('Ctrl Pts',(0.663382628119203,-0.244251601209411,
0.722929908501543));
#22514=CARTESIAN_POINT('Ctrl Pts',(0.679352081686668,-0.246942143572133,
0.707917883896095));
#22515=CARTESIAN_POINT('Ctrl Pts',(0.707917883896095,-0.246942143572133,
0.679352081686668));
#22516=CARTESIAN_POINT('Ctrl Pts',(0.722929908501543,-0.244251601209411,
0.663382628119203));
#22517=CARTESIAN_POINT('Ctrl Pts',(0.750785745543687,-0.232861760990032,
0.631684198665439));
#22518=CARTESIAN_POINT('Ctrl Pts',(0.763642258217232,-0.224161999508995,
0.615966552324775));
#22519=CARTESIAN_POINT('Ctrl Pts',(0.78555112003688,-0.203463743702801,
0.587792702767295));
#22520=CARTESIAN_POINT('Ctrl Pts',(0.795684265985088,-0.190326085855194,
0.573915184558108));
#22521=CARTESIAN_POINT('Ctrl Pts',(0.813159949759,-0.15976606450048,0.548874290046456));
#22522=CARTESIAN_POINT('Ctrl Pts',(0.820511285096538,-0.142345102874864,
0.537715343527944));
#22523=CARTESIAN_POINT('Ctrl Pts',(0.833661031856294,-0.099930567888331,
0.517157748491653));
#22524=CARTESIAN_POINT('Ctrl Pts',(0.838633903678357,-0.0740444353928835,
0.508899795931835));
#22525=CARTESIAN_POINT('Ctrl Pts',(0.841298510752801,-0.0476299999999999,
0.504455939115715));
#22526=CARTESIAN_POINT('',(0.528110872004958,-0.04763,0.871530771444223));
#22527=CARTESIAN_POINT('Origin',(0.707106781186547,-0.04763,0.707106781186548));
#22528=CARTESIAN_POINT('',(0.871530771444223,-0.04763,0.528110872004959));
#22529=CARTESIAN_POINT('Ctrl Pts',(0.871530771444223,-0.0476300000000001,
0.528110872004958));
#22530=CARTESIAN_POINT('Ctrl Pts',(0.87014664509073,-0.0609922781173483,
0.530395067942936));
#22531=CARTESIAN_POINT('Ctrl Pts',(0.868149331745851,-0.0742967091364493,
0.533674141594226));
#22532=CARTESIAN_POINT('Ctrl Pts',(0.85981294420286,-0.115492077056649,
0.54708917182331));
#22533=CARTESIAN_POINT('Ctrl Pts',(0.850993704737257,-0.141695629206859,
0.560922177770136));
#22534=CARTESIAN_POINT('Ctrl Pts',(0.830754510485543,-0.181890537957859,
0.590422647829571));
#22535=CARTESIAN_POINT('Ctrl Pts',(0.816896541396381,-0.201072148666545,
0.609616703125488));
#22536=CARTESIAN_POINT('Ctrl Pts',(0.792310597819928,-0.223955109275652,
0.641117951819998));
#22537=CARTESIAN_POINT('Ctrl Pts',(0.779109323683612,-0.232742381310829,
0.657208095763053));
#22538=CARTESIAN_POINT('Ctrl Pts',(0.750552691816206,-0.244234834628584,
0.68964083160521));
#22539=CARTESIAN_POINT('Ctrl Pts',(0.735185187071673,-0.246942143572133,
0.705971972091755));
#22540=CARTESIAN_POINT('Ctrl Pts',(0.705971972091754,-0.246942143572133,
0.735185187071673));
#22541=CARTESIAN_POINT('Ctrl Pts',(0.689640831605209,-0.244234834628584,
0.750552691816206));
#22542=CARTESIAN_POINT('Ctrl Pts',(0.657208095763052,-0.232742381310829,
0.779109323683612));
#22543=CARTESIAN_POINT('Ctrl Pts',(0.641117951819998,-0.223955109275652,
0.792310597819928));
#22544=CARTESIAN_POINT('Ctrl Pts',(0.609616703125487,-0.201072148666545,
0.816896541396382));
#22545=CARTESIAN_POINT('Ctrl Pts',(0.590422647829571,-0.181890537957858,
0.830754510485544));
#22546=CARTESIAN_POINT('Ctrl Pts',(0.560922177770135,-0.141695629206858,
0.850993704737257));
#22547=CARTESIAN_POINT('Ctrl Pts',(0.547089171823309,-0.115492077056649,
0.859812944202861));
#22548=CARTESIAN_POINT('Ctrl Pts',(0.533674141594226,-0.0742967091364491,
0.868149331745852));
#22549=CARTESIAN_POINT('Ctrl Pts',(0.530395067942936,-0.0609922781173483,
0.870146645090731));
#22550=CARTESIAN_POINT('Ctrl Pts',(0.528110872004958,-0.0476300000000001,
0.871530771444223));
#22551=CARTESIAN_POINT('Origin',(0.707106781186547,-0.04763,0.707106781186548));
#22552=CARTESIAN_POINT('Origin',(0.,-0.166705,0.));
#22553=CARTESIAN_POINT('',(0.242834539687906,-0.04763,0.989696097314));
#22554=CARTESIAN_POINT('Origin',(0.,-0.04763,0.));
#22555=CARTESIAN_POINT('',(-0.242834539687907,-0.04763,0.989696097314));
#22556=CARTESIAN_POINT('Ctrl Pts',(0.242834539687906,-0.04763,0.989696097314));
#22557=CARTESIAN_POINT('Ctrl Pts',(0.24024064412003,-0.0609922781173483,
0.990332542620729));
#22558=CARTESIAN_POINT('Ctrl Pts',(0.236509675094874,-0.0742967091364492,
0.991238884025248));
#22559=CARTESIAN_POINT('Ctrl Pts',(0.221129100087819,-0.115492077056649,
0.994830026707808));
#22560=CARTESIAN_POINT('Ctrl Pts',(0.205111543747588,-0.141695629206859,
0.998375294985966));
#22561=CARTESIAN_POINT('Ctrl Pts',(0.169940289819232,-0.181890537957859,
1.00492400591205));
#22562=CARTESIAN_POINT('Ctrl Pts',(0.1465689792446,-0.201072148666545,1.00869718865384));
#22563=CARTESIAN_POINT('Ctrl Pts',(0.106909345252087,-0.223955109275652,
1.01358704779679));
#22564=CARTESIAN_POINT('Ctrl Pts',(0.0861971848975941,-0.232742381310829,
1.0156297872271));
#22565=CARTESIAN_POINT('Ctrl Pts',(0.0430711894098822,-0.244234834628584,
1.01837060663223));
#22566=CARTESIAN_POINT('Ctrl Pts',(0.0206568624125605,-0.246942143572133,
1.019052));
#22567=CARTESIAN_POINT('Ctrl Pts',(-0.0206568624125608,-0.246942143572133,
1.019052));
#22568=CARTESIAN_POINT('Ctrl Pts',(-0.0430711894098825,-0.244234834628584,
1.01837060663223));
#22569=CARTESIAN_POINT('Ctrl Pts',(-0.0861971848975943,-0.232742381310829,
1.0156297872271));
#22570=CARTESIAN_POINT('Ctrl Pts',(-0.106909345252088,-0.223955109275652,
1.01358704779679));
#22571=CARTESIAN_POINT('Ctrl Pts',(-0.1465689792446,-0.201072148666545,
1.00869718865384));
#22572=CARTESIAN_POINT('Ctrl Pts',(-0.169940289819232,-0.181890537957859,
1.00492400591205));
#22573=CARTESIAN_POINT('Ctrl Pts',(-0.205111543747588,-0.141695629206859,
0.998375294985966));
#22574=CARTESIAN_POINT('Ctrl Pts',(-0.221129100087819,-0.115492077056649,
0.994830026707808));
#22575=CARTESIAN_POINT('Ctrl Pts',(-0.236509675094875,-0.0742967091364493,
0.991238884025248));
#22576=CARTESIAN_POINT('Ctrl Pts',(-0.24024064412003,-0.0609922781173483,
0.990332542620729));
#22577=CARTESIAN_POINT('Ctrl Pts',(-0.242834539687907,-0.04763,0.989696097314));
#22578=CARTESIAN_POINT('',(-0.528110872004959,-0.04763,0.871530771444223));
#22579=CARTESIAN_POINT('Origin',(0.,-0.04763,0.));
#22580=CARTESIAN_POINT('',(-0.871530771444223,-0.04763,0.528110872004958));
#22581=CARTESIAN_POINT('Ctrl Pts',(-0.528110872004958,-0.0476300000000001,
0.871530771444223));
#22582=CARTESIAN_POINT('Ctrl Pts',(-0.530395067942936,-0.0609922781173484,
0.87014664509073));
#22583=CARTESIAN_POINT('Ctrl Pts',(-0.533674141594226,-0.0742967091364493,
0.868149331745851));
#22584=CARTESIAN_POINT('Ctrl Pts',(-0.54708917182331,-0.115492077056649,
0.85981294420286));
#22585=CARTESIAN_POINT('Ctrl Pts',(-0.560922177770136,-0.141695629206859,
0.850993704737257));
#22586=CARTESIAN_POINT('Ctrl Pts',(-0.590422647829571,-0.181890537957859,
0.830754510485543));
#22587=CARTESIAN_POINT('Ctrl Pts',(-0.609616703125488,-0.201072148666545,
0.816896541396381));
#22588=CARTESIAN_POINT('Ctrl Pts',(-0.641117951819998,-0.223955109275652,
0.792310597819928));
#22589=CARTESIAN_POINT('Ctrl Pts',(-0.657208095763053,-0.232742381310829,
0.779109323683611));
#22590=CARTESIAN_POINT('Ctrl Pts',(-0.68964083160521,-0.244234834628584,
0.750552691816205));
#22591=CARTESIAN_POINT('Ctrl Pts',(-0.705971972091755,-0.246942143572133,
0.735185187071673));
#22592=CARTESIAN_POINT('Ctrl Pts',(-0.735185187071673,-0.246942143572133,
0.705971972091754));
#22593=CARTESIAN_POINT('Ctrl Pts',(-0.750552691816206,-0.244234834628584,
0.689640831605209));
#22594=CARTESIAN_POINT('Ctrl Pts',(-0.779109323683612,-0.232742381310829,
0.657208095763052));
#22595=CARTESIAN_POINT('Ctrl Pts',(-0.792310597819928,-0.223955109275652,
0.641117951819998));
#22596=CARTESIAN_POINT('Ctrl Pts',(-0.816896541396382,-0.201072148666545,
0.609616703125487));
#22597=CARTESIAN_POINT('Ctrl Pts',(-0.830754510485544,-0.181890537957858,
0.590422647829571));
#22598=CARTESIAN_POINT('Ctrl Pts',(-0.850993704737257,-0.141695629206858,
0.560922177770135));
#22599=CARTESIAN_POINT('Ctrl Pts',(-0.859812944202861,-0.115492077056649,
0.547089171823309));
#22600=CARTESIAN_POINT('Ctrl Pts',(-0.868149331745852,-0.0742967091364491,
0.533674141594226));
#22601=CARTESIAN_POINT('Ctrl Pts',(-0.870146645090731,-0.0609922781173483,
0.530395067942936));
#22602=CARTESIAN_POINT('Ctrl Pts',(-0.871530771444223,-0.04763,0.528110872004958));
#22603=CARTESIAN_POINT('',(-0.989696097314,-0.04763,0.242834539687906));
#22604=CARTESIAN_POINT('Origin',(0.,-0.04763,0.));
#22605=CARTESIAN_POINT('',(-1.019052,-0.246942143572133,1.248489836334E-16));
#22606=CARTESIAN_POINT('Ctrl Pts',(-0.989696097314,-0.04763,0.242834539687906));
#22607=CARTESIAN_POINT('Ctrl Pts',(-0.990332542620729,-0.0609922781173483,
0.24024064412003));
#22608=CARTESIAN_POINT('Ctrl Pts',(-0.991238884025248,-0.0742967091364492,
0.236509675094874));
#22609=CARTESIAN_POINT('Ctrl Pts',(-0.994830026707808,-0.115492077056649,
0.221129100087819));
#22610=CARTESIAN_POINT('Ctrl Pts',(-0.998375294985966,-0.141695629206859,
0.205111543747588));
#22611=CARTESIAN_POINT('Ctrl Pts',(-1.00492400591205,-0.181890537957859,
0.169940289819232));
#22612=CARTESIAN_POINT('Ctrl Pts',(-1.00869718865384,-0.201072148666545,
0.1465689792446));
#22613=CARTESIAN_POINT('Ctrl Pts',(-1.01358704779679,-0.223955109275652,
0.106909345252088));
#22614=CARTESIAN_POINT('Ctrl Pts',(-1.0156297872271,-0.232742381310829,
0.0861971848975944));
#22615=CARTESIAN_POINT('Ctrl Pts',(-1.01837060663223,-0.244234834628584,
0.0430711894098825));
#22616=CARTESIAN_POINT('Ctrl Pts',(-1.019052,-0.246942143572133,0.0206568624125608));
#22617=CARTESIAN_POINT('Ctrl Pts',(-1.019052,-0.246942143572133,1.2490009027033E-16));
#22618=CARTESIAN_POINT('',(-1.019052,-0.28578,1.24797876996471E-16));
#22619=CARTESIAN_POINT('',(-1.019052,-0.166705,1.24797876996471E-16));
#22620=CARTESIAN_POINT('Origin',(0.,-0.28578,0.));
#22621=CARTESIAN_POINT('',(-0.989696097314,-0.04763,-0.242834539687906));
#22622=CARTESIAN_POINT('Ctrl Pts',(-1.019052,-0.246942143572133,1.2490009027033E-16));
#22623=CARTESIAN_POINT('Ctrl Pts',(-1.019052,-0.246942143572133,-0.0206568624125605));
#22624=CARTESIAN_POINT('Ctrl Pts',(-1.01837060663223,-0.244234834628584,
-0.0430711894098822));
#22625=CARTESIAN_POINT('Ctrl Pts',(-1.0156297872271,-0.232742381310829,
-0.0861971848975941));
#22626=CARTESIAN_POINT('Ctrl Pts',(-1.01358704779679,-0.223955109275652,
-0.106909345252087));
#22627=CARTESIAN_POINT('Ctrl Pts',(-1.00869718865384,-0.201072148666546,
-0.1465689792446));
#22628=CARTESIAN_POINT('Ctrl Pts',(-1.00492400591205,-0.181890537957859,
-0.169940289819232));
#22629=CARTESIAN_POINT('Ctrl Pts',(-0.998375294985966,-0.141695629206859,
-0.205111543747588));
#22630=CARTESIAN_POINT('Ctrl Pts',(-0.994830026707808,-0.11549207705665,
-0.221129100087819));
#22631=CARTESIAN_POINT('Ctrl Pts',(-0.991238884025248,-0.0742967091364495,
-0.236509675094874));
#22632=CARTESIAN_POINT('Ctrl Pts',(-0.990332542620729,-0.0609922781173484,
-0.24024064412003));
#22633=CARTESIAN_POINT('Ctrl Pts',(-0.989696097314,-0.0476300000000001,
-0.242834539687907));
#22634=CARTESIAN_POINT('',(-0.871530771444223,-0.04763,-0.528110872004958));
#22635=CARTESIAN_POINT('Origin',(0.,-0.04763,0.));
#22636=CARTESIAN_POINT('',(-0.528110872004958,-0.04763,-0.871530771444223));
#22637=CARTESIAN_POINT('Ctrl Pts',(-0.871530771444223,-0.0476300000000001,
-0.528110872004958));
#22638=CARTESIAN_POINT('Ctrl Pts',(-0.87014664509073,-0.0609922781173484,
-0.530395067942936));
#22639=CARTESIAN_POINT('Ctrl Pts',(-0.868149331745851,-0.0742967091364494,
-0.533674141594226));
#22640=CARTESIAN_POINT('Ctrl Pts',(-0.85981294420286,-0.115492077056649,
-0.54708917182331));
#22641=CARTESIAN_POINT('Ctrl Pts',(-0.850993704737257,-0.141695629206859,
-0.560922177770136));
#22642=CARTESIAN_POINT('Ctrl Pts',(-0.830754510485543,-0.181890537957859,
-0.590422647829571));
#22643=CARTESIAN_POINT('Ctrl Pts',(-0.816896541396381,-0.201072148666546,
-0.609616703125488));
#22644=CARTESIAN_POINT('Ctrl Pts',(-0.792310597819928,-0.223955109275652,
-0.641117951819999));
#22645=CARTESIAN_POINT('Ctrl Pts',(-0.779109323683611,-0.232742381310829,
-0.657208095763053));
#22646=CARTESIAN_POINT('Ctrl Pts',(-0.750552691816205,-0.244234834628584,
-0.68964083160521));
#22647=CARTESIAN_POINT('Ctrl Pts',(-0.735185187071673,-0.246942143572133,
-0.705971972091755));
#22648=CARTESIAN_POINT('Ctrl Pts',(-0.705971972091754,-0.246942143572133,
-0.735185187071673));
#22649=CARTESIAN_POINT('Ctrl Pts',(-0.68964083160521,-0.244234834628584,
-0.750552691816206));
#22650=CARTESIAN_POINT('Ctrl Pts',(-0.657208095763052,-0.232742381310829,
-0.779109323683612));
#22651=CARTESIAN_POINT('Ctrl Pts',(-0.641117951819998,-0.223955109275652,
-0.792310597819928));
#22652=CARTESIAN_POINT('Ctrl Pts',(-0.609616703125488,-0.201072148666545,
-0.816896541396381));
#22653=CARTESIAN_POINT('Ctrl Pts',(-0.590422647829571,-0.181890537957859,
-0.830754510485543));
#22654=CARTESIAN_POINT('Ctrl Pts',(-0.560922177770136,-0.141695629206859,
-0.850993704737257));
#22655=CARTESIAN_POINT('Ctrl Pts',(-0.54708917182331,-0.115492077056649,
-0.85981294420286));
#22656=CARTESIAN_POINT('Ctrl Pts',(-0.533674141594226,-0.0742967091364494,
-0.868149331745852));
#22657=CARTESIAN_POINT('Ctrl Pts',(-0.530395067942936,-0.0609922781173484,
-0.870146645090731));
#22658=CARTESIAN_POINT('Ctrl Pts',(-0.528110872004958,-0.0476300000000001,
-0.871530771444223));
#22659=CARTESIAN_POINT('',(-0.242834539687906,-0.04763,-0.989696097314));
#22660=CARTESIAN_POINT('Origin',(0.,-0.04763,0.));
#22661=CARTESIAN_POINT('',(0.242834539687906,-0.04763,-0.989696097314));
#22662=CARTESIAN_POINT('Ctrl Pts',(-0.242834539687907,-0.04763,-0.989696097314));
#22663=CARTESIAN_POINT('Ctrl Pts',(-0.24024064412003,-0.0609922781173483,
-0.990332542620729));
#22664=CARTESIAN_POINT('Ctrl Pts',(-0.236509675094874,-0.0742967091364493,
-0.991238884025248));
#22665=CARTESIAN_POINT('Ctrl Pts',(-0.221129100087819,-0.115492077056649,
-0.994830026707808));
#22666=CARTESIAN_POINT('Ctrl Pts',(-0.205111543747588,-0.141695629206859,
-0.998375294985966));
#22667=CARTESIAN_POINT('Ctrl Pts',(-0.169940289819232,-0.181890537957859,
-1.00492400591205));
#22668=CARTESIAN_POINT('Ctrl Pts',(-0.1465689792446,-0.201072148666545,
-1.00869718865384));
#22669=CARTESIAN_POINT('Ctrl Pts',(-0.106909345252087,-0.223955109275652,
-1.01358704779679));
#22670=CARTESIAN_POINT('Ctrl Pts',(-0.0861971848975942,-0.232742381310829,
-1.0156297872271));
#22671=CARTESIAN_POINT('Ctrl Pts',(-0.0430711894098823,-0.244234834628584,
-1.01837060663223));
#22672=CARTESIAN_POINT('Ctrl Pts',(-0.0206568624125606,-0.246942143572133,
-1.019052));
#22673=CARTESIAN_POINT('Ctrl Pts',(0.0206568624125607,-0.246942143572133,
-1.019052));
#22674=CARTESIAN_POINT('Ctrl Pts',(0.0430711894098824,-0.244234834628584,
-1.01837060663223));
#22675=CARTESIAN_POINT('Ctrl Pts',(0.0861971848975943,-0.232742381310829,
-1.0156297872271));
#22676=CARTESIAN_POINT('Ctrl Pts',(0.106909345252088,-0.223955109275652,
-1.01358704779679));
#22677=CARTESIAN_POINT('Ctrl Pts',(0.1465689792446,-0.201072148666545,-1.00869718865384));
#22678=CARTESIAN_POINT('Ctrl Pts',(0.169940289819232,-0.181890537957859,
-1.00492400591205));
#22679=CARTESIAN_POINT('Ctrl Pts',(0.205111543747588,-0.141695629206859,
-0.998375294985966));
#22680=CARTESIAN_POINT('Ctrl Pts',(0.221129100087819,-0.115492077056649,
-0.994830026707808));
#22681=CARTESIAN_POINT('Ctrl Pts',(0.236509675094874,-0.0742967091364493,
-0.991238884025248));
#22682=CARTESIAN_POINT('Ctrl Pts',(0.24024064412003,-0.0609922781173484,
-0.990332542620729));
#22683=CARTESIAN_POINT('Ctrl Pts',(0.242834539687907,-0.04763,-0.989696097314));
#22684=CARTESIAN_POINT('',(0.528110872004958,-0.04763,-0.871530771444223));
#22685=CARTESIAN_POINT('Origin',(0.,-0.04763,0.));
#22686=CARTESIAN_POINT('',(0.871530771444223,-0.04763,-0.528110872004958));
#22687=CARTESIAN_POINT('Ctrl Pts',(0.528110872004958,-0.0476300000000001,
-0.871530771444223));
#22688=CARTESIAN_POINT('Ctrl Pts',(0.530395067942936,-0.0609922781173484,
-0.870146645090731));
#22689=CARTESIAN_POINT('Ctrl Pts',(0.533674141594226,-0.0742967091364493,
-0.868149331745851));
#22690=CARTESIAN_POINT('Ctrl Pts',(0.54708917182331,-0.115492077056649,
-0.85981294420286));
#22691=CARTESIAN_POINT('Ctrl Pts',(0.560922177770136,-0.141695629206859,
-0.850993704737257));
#22692=CARTESIAN_POINT('Ctrl Pts',(0.590422647829571,-0.181890537957859,
-0.830754510485543));
#22693=CARTESIAN_POINT('Ctrl Pts',(0.609616703125488,-0.201072148666545,
-0.816896541396381));
#22694=CARTESIAN_POINT('Ctrl Pts',(0.641117951819998,-0.223955109275652,
-0.792310597819928));
#22695=CARTESIAN_POINT('Ctrl Pts',(0.657208095763053,-0.232742381310829,
-0.779109323683612));
#22696=CARTESIAN_POINT('Ctrl Pts',(0.68964083160521,-0.244234834628584,
-0.750552691816206));
#22697=CARTESIAN_POINT('Ctrl Pts',(0.705971972091755,-0.246942143572133,
-0.735185187071673));
#22698=CARTESIAN_POINT('Ctrl Pts',(0.735185187071673,-0.246942143572133,
-0.705971972091754));
#22699=CARTESIAN_POINT('Ctrl Pts',(0.750552691816206,-0.244234834628584,
-0.68964083160521));
#22700=CARTESIAN_POINT('Ctrl Pts',(0.779109323683612,-0.232742381310829,
-0.657208095763053));
#22701=CARTESIAN_POINT('Ctrl Pts',(0.792310597819928,-0.223955109275652,
-0.641117951819998));
#22702=CARTESIAN_POINT('Ctrl Pts',(0.816896541396381,-0.201072148666545,
-0.609616703125488));
#22703=CARTESIAN_POINT('Ctrl Pts',(0.830754510485543,-0.181890537957859,
-0.590422647829571));
#22704=CARTESIAN_POINT('Ctrl Pts',(0.850993704737257,-0.141695629206859,
-0.560922177770136));
#22705=CARTESIAN_POINT('Ctrl Pts',(0.85981294420286,-0.115492077056649,
-0.54708917182331));
#22706=CARTESIAN_POINT('Ctrl Pts',(0.868149331745851,-0.0742967091364493,
-0.533674141594226));
#22707=CARTESIAN_POINT('Ctrl Pts',(0.870146645090731,-0.0609922781173484,
-0.530395067942936));
#22708=CARTESIAN_POINT('Ctrl Pts',(0.871530771444223,-0.0476300000000001,
-0.528110872004958));
#22709=CARTESIAN_POINT('',(0.989696097314,-0.04763,-0.242834539687906));
#22710=CARTESIAN_POINT('Origin',(0.,-0.04763,0.));
#22711=CARTESIAN_POINT('',(0.989696097314,-0.04763,0.242834539687906));
#22712=CARTESIAN_POINT('Ctrl Pts',(0.989696097314,-0.04763,-0.242834539687907));
#22713=CARTESIAN_POINT('Ctrl Pts',(0.990332542620729,-0.0609922781173483,
-0.24024064412003));
#22714=CARTESIAN_POINT('Ctrl Pts',(0.991238884025248,-0.0742967091364493,
-0.236509675094874));
#22715=CARTESIAN_POINT('Ctrl Pts',(0.994830026707808,-0.115492077056649,
-0.221129100087819));
#22716=CARTESIAN_POINT('Ctrl Pts',(0.998375294985966,-0.141695629206859,
-0.205111543747588));
#22717=CARTESIAN_POINT('Ctrl Pts',(1.00492400591205,-0.181890537957859,
-0.169940289819232));
#22718=CARTESIAN_POINT('Ctrl Pts',(1.00869718865384,-0.201072148666545,
-0.1465689792446));
#22719=CARTESIAN_POINT('Ctrl Pts',(1.01358704779679,-0.223955109275652,
-0.106909345252087));
#22720=CARTESIAN_POINT('Ctrl Pts',(1.0156297872271,-0.232742381310829,-0.0861971848975942));
#22721=CARTESIAN_POINT('Ctrl Pts',(1.01837060663223,-0.244234834628584,
-0.0430711894098823));
#22722=CARTESIAN_POINT('Ctrl Pts',(1.019052,-0.246942143572133,-0.0206568624125607));
#22723=CARTESIAN_POINT('Ctrl Pts',(1.019052,-0.246942143572133,0.0206568624125607));
#22724=CARTESIAN_POINT('Ctrl Pts',(1.01837060663223,-0.244234834628584,
0.0430711894098823));
#22725=CARTESIAN_POINT('Ctrl Pts',(1.0156297872271,-0.232742381310829,0.0861971848975942));
#22726=CARTESIAN_POINT('Ctrl Pts',(1.01358704779679,-0.223955109275652,
0.106909345252087));
#22727=CARTESIAN_POINT('Ctrl Pts',(1.00869718865384,-0.201072148666545,
0.1465689792446));
#22728=CARTESIAN_POINT('Ctrl Pts',(1.00492400591205,-0.181890537957859,
0.169940289819232));
#22729=CARTESIAN_POINT('Ctrl Pts',(0.998375294985966,-0.141695629206859,
0.205111543747588));
#22730=CARTESIAN_POINT('Ctrl Pts',(0.994830026707808,-0.115492077056649,
0.221129100087819));
#22731=CARTESIAN_POINT('Ctrl Pts',(0.991238884025248,-0.0742967091364492,
0.236509675094874));
#22732=CARTESIAN_POINT('Ctrl Pts',(0.990332542620729,-0.0609922781173483,
0.24024064412003));
#22733=CARTESIAN_POINT('Ctrl Pts',(0.989696097314,-0.04763,0.242834539687907));
#22734=CARTESIAN_POINT('Origin',(0.,-0.04763,0.));
#22735=CARTESIAN_POINT('Origin',(0.,-0.04763,0.));
#22736=CARTESIAN_POINT('',(0.238183666596899,-0.04763,0.951592097314));
#22737=CARTESIAN_POINT('Origin',(0.,-0.04763,0.));
#22738=CARTESIAN_POINT('Origin',(-1.94289029309402E-16,-0.04763,1.));
#22739=CARTESIAN_POINT('Origin',(-1.94289029309402E-16,0.,1.));
#22740=CARTESIAN_POINT('',(-0.2381836665969,-0.04763,0.951592097314));
#22741=CARTESIAN_POINT('Ctrl Pts',(-0.238183666596899,-0.0476299999999999,
0.951592097314));
#22742=CARTESIAN_POINT('Ctrl Pts',(-0.233157223576062,-0.0740444353928835,
0.952850216871763));
#22743=CARTESIAN_POINT('Ctrl Pts',(-0.223801617934946,-0.0999305678883309,
0.955173119738174));
#22744=CARTESIAN_POINT('Ctrl Pts',(-0.199966927975188,-0.142345102874864,
0.960411259488514));
#22745=CARTESIAN_POINT('Ctrl Pts',(-0.1868781821531,-0.159766064500479,
0.963103647174702));
#22746=CARTESIAN_POINT('Ctrl Pts',(-0.15681442133453,-0.190326085855194,
0.968453058988463));
#22747=CARTESIAN_POINT('Ctrl Pts',(-0.139836317888043,-0.203463743702801,
0.971100730005489));
#22748=CARTESIAN_POINT('Ctrl Pts',(-0.104422493053067,-0.224161999508995,
0.975530745318961));
#22749=CARTESIAN_POINT('Ctrl Pts',(-0.0842175114474176,-0.232861760990032,
0.977553872336861));
#22750=CARTESIAN_POINT('Ctrl Pts',(-0.0421062857595701,-0.244251601209411,
0.980270995488453));
#22751=CARTESIAN_POINT('Ctrl Pts',(-0.0201990724523197,-0.246942143572133,
0.980948));
#22752=CARTESIAN_POINT('Ctrl Pts',(0.020199072452319,-0.246942143572133,
0.980948));
#22753=CARTESIAN_POINT('Ctrl Pts',(0.0421062857595694,-0.244251601209411,
0.980270995488454));
#22754=CARTESIAN_POINT('Ctrl Pts',(0.0842175114474169,-0.232861760990032,
0.977553872336861));
#22755=CARTESIAN_POINT('Ctrl Pts',(0.104422493053067,-0.224161999508995,
0.975530745318961));
#22756=CARTESIAN_POINT('Ctrl Pts',(0.139836317888042,-0.203463743702801,
0.971100730005489));
#22757=CARTESIAN_POINT('Ctrl Pts',(0.15681442133453,-0.190326085855194,
0.968453058988463));
#22758=CARTESIAN_POINT('Ctrl Pts',(0.1868781821531,-0.15976606450048,0.963103647174702));
#22759=CARTESIAN_POINT('Ctrl Pts',(0.199966927975188,-0.142345102874864,
0.960411259488514));
#22760=CARTESIAN_POINT('Ctrl Pts',(0.223801617934945,-0.0999305678883309,
0.955173119738174));
#22761=CARTESIAN_POINT('Ctrl Pts',(0.233157223576061,-0.0740444353928835,
0.952850216871763));
#22762=CARTESIAN_POINT('Ctrl Pts',(0.238183666596899,-0.0476299999999999,
0.951592097314));
#22763=CARTESIAN_POINT('Origin',(-1.94289029309402E-16,-0.04763,1.));
#22764=CARTESIAN_POINT('Origin',(0.,-0.04763,0.));
#22765=CARTESIAN_POINT('',(-0.504455939115715,-0.04763,0.841298510752802));
#22766=CARTESIAN_POINT('Origin',(0.,-0.04763,0.));
#22767=CARTESIAN_POINT('Origin',(-0.707106781186548,-0.04763,0.707106781186547));
#22768=CARTESIAN_POINT('Origin',(-0.707106781186548,0.,0.707106781186547));
#22769=CARTESIAN_POINT('',(-0.841298510752802,-0.04763,0.504455939115715));
#22770=CARTESIAN_POINT('Ctrl Pts',(-0.841298510752802,-0.04763,0.504455939115715));
#22771=CARTESIAN_POINT('Ctrl Pts',(-0.838633903678357,-0.0740444353928835,
0.508899795931835));
#22772=CARTESIAN_POINT('Ctrl Pts',(-0.833661031856294,-0.0999305678883309,
0.517157748491652));
#22773=CARTESIAN_POINT('Ctrl Pts',(-0.820511285096538,-0.142345102874864,
0.537715343527944));
#22774=CARTESIAN_POINT('Ctrl Pts',(-0.813159949759,-0.159766064500479,0.548874290046456));
#22775=CARTESIAN_POINT('Ctrl Pts',(-0.795684265985089,-0.190326085855194,
0.573915184558107));
#22776=CARTESIAN_POINT('Ctrl Pts',(-0.78555112003688,-0.203463743702801,
0.587792702767295));
#22777=CARTESIAN_POINT('Ctrl Pts',(-0.763642258217233,-0.224161999508995,
0.615966552324775));
#22778=CARTESIAN_POINT('Ctrl Pts',(-0.750785745543687,-0.232861760990032,
0.631684198665438));
#22779=CARTESIAN_POINT('Ctrl Pts',(-0.722929908501543,-0.244251601209411,
0.663382628119203));
#22780=CARTESIAN_POINT('Ctrl Pts',(-0.707917883896095,-0.246942143572133,
0.679352081686668));
#22781=CARTESIAN_POINT('Ctrl Pts',(-0.679352081686668,-0.246942143572133,
0.707917883896095));
#22782=CARTESIAN_POINT('Ctrl Pts',(-0.663382628119203,-0.244251601209411,
0.722929908501544));
#22783=CARTESIAN_POINT('Ctrl Pts',(-0.631684198665438,-0.232861760990031,
0.750785745543687));
#22784=CARTESIAN_POINT('Ctrl Pts',(-0.615966552324775,-0.224161999508995,
0.763642258217233));
#22785=CARTESIAN_POINT('Ctrl Pts',(-0.587792702767295,-0.203463743702801,
0.78555112003688));
#22786=CARTESIAN_POINT('Ctrl Pts',(-0.573915184558107,-0.190326085855194,
0.795684265985088));
#22787=CARTESIAN_POINT('Ctrl Pts',(-0.548874290046456,-0.159766064500479,
0.813159949759));
#22788=CARTESIAN_POINT('Ctrl Pts',(-0.537715343527944,-0.142345102874864,
0.820511285096538));
#22789=CARTESIAN_POINT('Ctrl Pts',(-0.517157748491652,-0.0999305678883309,
0.833661031856294));
#22790=CARTESIAN_POINT('Ctrl Pts',(-0.508899795931835,-0.0740444353928835,
0.838633903678357));
#22791=CARTESIAN_POINT('Ctrl Pts',(-0.504455939115716,-0.04763,0.841298510752801));
#22792=CARTESIAN_POINT('Origin',(-0.707106781186548,-0.04763,0.707106781186547));
#22793=CARTESIAN_POINT('Origin',(0.,-0.04763,0.));
#22794=CARTESIAN_POINT('',(-0.951592097314,-0.04763,0.238183666596899));
#22795=CARTESIAN_POINT('Origin',(0.,-0.04763,0.));
#22796=CARTESIAN_POINT('Origin',(-1.,-0.04763,-1.11022302462516E-16));
#22797=CARTESIAN_POINT('Origin',(-1.,0.,-1.11022302462516E-16));
#22798=CARTESIAN_POINT('',(-0.951592097314,-0.04763,-0.2381836665969));
#22799=CARTESIAN_POINT('',(-0.980948,-0.246942143572133,1.08514323328844E-18));
#22800=CARTESIAN_POINT('Ctrl Pts',(-0.951592097314,-0.04763,-0.238183666596899));
#22801=CARTESIAN_POINT('Ctrl Pts',(-0.952850216871763,-0.0740444353928835,
-0.233157223576062));
#22802=CARTESIAN_POINT('Ctrl Pts',(-0.955173119738174,-0.0999305678883309,
-0.223801617934946));
#22803=CARTESIAN_POINT('Ctrl Pts',(-0.960411259488514,-0.142345102874864,
-0.199966927975188));
#22804=CARTESIAN_POINT('Ctrl Pts',(-0.963103647174702,-0.159766064500479,
-0.1868781821531));
#22805=CARTESIAN_POINT('Ctrl Pts',(-0.968453058988463,-0.190326085855194,
-0.15681442133453));
#22806=CARTESIAN_POINT('Ctrl Pts',(-0.971100730005489,-0.203463743702801,
-0.139836317888043));
#22807=CARTESIAN_POINT('Ctrl Pts',(-0.975530745318961,-0.224161999508995,
-0.104422493053067));
#22808=CARTESIAN_POINT('Ctrl Pts',(-0.977553872336861,-0.232861760990032,
-0.0842175114474175));
#22809=CARTESIAN_POINT('Ctrl Pts',(-0.980270995488453,-0.244251601209411,
-0.0421062857595699));
#22810=CARTESIAN_POINT('Ctrl Pts',(-0.980948,-0.246942143572133,-0.0201990724523195));
#22811=CARTESIAN_POINT('Ctrl Pts',(-0.980948,-0.246942143572133,-1.17961196366423E-16));
#22812=CARTESIAN_POINT('Origin',(-1.,-0.04763,-1.11022302462516E-16));
#22813=CARTESIAN_POINT('Ctrl Pts',(-0.980948,-0.246942143572133,-1.17961196366423E-16));
#22814=CARTESIAN_POINT('Ctrl Pts',(-0.980948,-0.246942143572133,0.0201990724523192));
#22815=CARTESIAN_POINT('Ctrl Pts',(-0.980270995488453,-0.244251601209411,
0.0421062857595695));
#22816=CARTESIAN_POINT('Ctrl Pts',(-0.977553872336861,-0.232861760990032,
0.0842175114474169));
#22817=CARTESIAN_POINT('Ctrl Pts',(-0.975530745318961,-0.224161999508995,
0.104422493053066));
#22818=CARTESIAN_POINT('Ctrl Pts',(-0.971100730005489,-0.203463743702801,
0.139836317888042));
#22819=CARTESIAN_POINT('Ctrl Pts',(-0.968453058988463,-0.190326085855194,
0.15681442133453));
#22820=CARTESIAN_POINT('Ctrl Pts',(-0.963103647174702,-0.15976606450048,
0.1868781821531));
#22821=CARTESIAN_POINT('Ctrl Pts',(-0.960411259488514,-0.142345102874864,
0.199966927975188));
#22822=CARTESIAN_POINT('Ctrl Pts',(-0.955173119738174,-0.099930567888331,
0.223801617934945));
#22823=CARTESIAN_POINT('Ctrl Pts',(-0.952850216871763,-0.0740444353928835,
0.233157223576061));
#22824=CARTESIAN_POINT('Ctrl Pts',(-0.951592097314,-0.04763,0.238183666596899));
#22825=CARTESIAN_POINT('Origin',(0.,-0.04763,0.));
#22826=CARTESIAN_POINT('',(-0.841298510752802,-0.04763,-0.504455939115715));
#22827=CARTESIAN_POINT('Origin',(0.,-0.04763,0.));
#22828=CARTESIAN_POINT('Origin',(-0.707106781186547,-0.04763,-0.707106781186548));
#22829=CARTESIAN_POINT('Origin',(-0.707106781186547,0.,-0.707106781186548));
#22830=CARTESIAN_POINT('',(-0.504455939115715,-0.04763,-0.841298510752802));
#22831=CARTESIAN_POINT('Ctrl Pts',(-0.504455939115715,-0.04763,-0.841298510752802));
#22832=CARTESIAN_POINT('Ctrl Pts',(-0.508899795931835,-0.0740444353928835,
-0.838633903678357));
#22833=CARTESIAN_POINT('Ctrl Pts',(-0.517157748491652,-0.0999305678883309,
-0.833661031856294));
#22834=CARTESIAN_POINT('Ctrl Pts',(-0.537715343527944,-0.142345102874864,
-0.820511285096538));
#22835=CARTESIAN_POINT('Ctrl Pts',(-0.548874290046456,-0.159766064500479,
-0.813159949759));
#22836=CARTESIAN_POINT('Ctrl Pts',(-0.573915184558107,-0.190326085855194,
-0.795684265985089));
#22837=CARTESIAN_POINT('Ctrl Pts',(-0.587792702767295,-0.203463743702801,
-0.78555112003688));
#22838=CARTESIAN_POINT('Ctrl Pts',(-0.615966552324775,-0.224161999508995,
-0.763642258217233));
#22839=CARTESIAN_POINT('Ctrl Pts',(-0.631684198665438,-0.232861760990032,
-0.750785745543687));
#22840=CARTESIAN_POINT('Ctrl Pts',(-0.663382628119203,-0.244251601209411,
-0.722929908501543));
#22841=CARTESIAN_POINT('Ctrl Pts',(-0.679352081686668,-0.246942143572133,
-0.707917883896095));
#22842=CARTESIAN_POINT('Ctrl Pts',(-0.707917883896095,-0.246942143572133,
-0.679352081686668));
#22843=CARTESIAN_POINT('Ctrl Pts',(-0.722929908501543,-0.244251601209411,
-0.663382628119203));
#22844=CARTESIAN_POINT('Ctrl Pts',(-0.750785745543687,-0.232861760990032,
-0.631684198665439));
#22845=CARTESIAN_POINT('Ctrl Pts',(-0.763642258217232,-0.224161999508995,
-0.615966552324775));
#22846=CARTESIAN_POINT('Ctrl Pts',(-0.78555112003688,-0.203463743702801,
-0.587792702767295));
#22847=CARTESIAN_POINT('Ctrl Pts',(-0.795684265985088,-0.190326085855194,
-0.573915184558107));
#22848=CARTESIAN_POINT('Ctrl Pts',(-0.813159949759,-0.15976606450048,-0.548874290046456));
#22849=CARTESIAN_POINT('Ctrl Pts',(-0.820511285096538,-0.142345102874864,
-0.537715343527944));
#22850=CARTESIAN_POINT('Ctrl Pts',(-0.833661031856294,-0.0999305678883311,
-0.517157748491652));
#22851=CARTESIAN_POINT('Ctrl Pts',(-0.838633903678357,-0.0740444353928836,
-0.508899795931835));
#22852=CARTESIAN_POINT('Ctrl Pts',(-0.841298510752801,-0.04763,-0.504455939115715));
#22853=CARTESIAN_POINT('Origin',(-0.707106781186547,-0.04763,-0.707106781186548));
#22854=CARTESIAN_POINT('Origin',(0.,-0.04763,0.));
#22855=CARTESIAN_POINT('',(-0.238183666596899,-0.04763,-0.951592097314));
#22856=CARTESIAN_POINT('Origin',(0.,-0.04763,0.));
#22857=CARTESIAN_POINT('Origin',(5.55111512312578E-17,-0.04763,-1.));
#22858=CARTESIAN_POINT('Origin',(5.55111512312578E-17,0.,-1.));
#22859=CARTESIAN_POINT('',(0.238183666596899,-0.04763,-0.951592097314));
#22860=CARTESIAN_POINT('Ctrl Pts',(0.238183666596899,-0.04763,-0.951592097314));
#22861=CARTESIAN_POINT('Ctrl Pts',(0.233157223576062,-0.0740444353928835,
-0.952850216871763));
#22862=CARTESIAN_POINT('Ctrl Pts',(0.223801617934946,-0.099930567888331,
-0.955173119738174));
#22863=CARTESIAN_POINT('Ctrl Pts',(0.199966927975188,-0.142345102874864,
-0.960411259488514));
#22864=CARTESIAN_POINT('Ctrl Pts',(0.1868781821531,-0.15976606450048,-0.963103647174702));
#22865=CARTESIAN_POINT('Ctrl Pts',(0.15681442133453,-0.190326085855194,
-0.968453058988463));
#22866=CARTESIAN_POINT('Ctrl Pts',(0.139836317888042,-0.203463743702801,
-0.971100730005489));
#22867=CARTESIAN_POINT('Ctrl Pts',(0.104422493053067,-0.224161999508995,
-0.975530745318961));
#22868=CARTESIAN_POINT('Ctrl Pts',(0.0842175114474173,-0.232861760990032,
-0.977553872336861));
#22869=CARTESIAN_POINT('Ctrl Pts',(0.0421062857595698,-0.244251601209411,
-0.980270995488453));
#22870=CARTESIAN_POINT('Ctrl Pts',(0.0201990724523194,-0.246942143572133,
-0.980948));
#22871=CARTESIAN_POINT('Ctrl Pts',(-0.0201990724523193,-0.246942143572133,
-0.980948));
#22872=CARTESIAN_POINT('Ctrl Pts',(-0.0421062857595697,-0.244251601209411,
-0.980270995488453));
#22873=CARTESIAN_POINT('Ctrl Pts',(-0.0842175114474171,-0.232861760990032,
-0.977553872336861));
#22874=CARTESIAN_POINT('Ctrl Pts',(-0.104422493053067,-0.224161999508995,
-0.975530745318961));
#22875=CARTESIAN_POINT('Ctrl Pts',(-0.139836317888042,-0.203463743702801,
-0.971100730005489));
#22876=CARTESIAN_POINT('Ctrl Pts',(-0.15681442133453,-0.190326085855194,
-0.968453058988463));
#22877=CARTESIAN_POINT('Ctrl Pts',(-0.1868781821531,-0.15976606450048,-0.963103647174702));
#22878=CARTESIAN_POINT('Ctrl Pts',(-0.199966927975188,-0.142345102874864,
-0.960411259488514));
#22879=CARTESIAN_POINT('Ctrl Pts',(-0.223801617934945,-0.099930567888331,
-0.955173119738174));
#22880=CARTESIAN_POINT('Ctrl Pts',(-0.233157223576062,-0.0740444353928835,
-0.952850216871763));
#22881=CARTESIAN_POINT('Ctrl Pts',(-0.238183666596899,-0.0476299999999999,
-0.951592097314));
#22882=CARTESIAN_POINT('Origin',(5.55111512312578E-17,-0.04763,-1.));
#22883=CARTESIAN_POINT('Origin',(0.,-0.04763,0.));
#22884=CARTESIAN_POINT('',(0.504455939115715,-0.04763,-0.841298510752802));
#22885=CARTESIAN_POINT('Origin',(0.,-0.04763,0.));
#22886=CARTESIAN_POINT('Origin',(0.707106781186548,-0.04763,-0.707106781186547));
#22887=CARTESIAN_POINT('Origin',(0.707106781186548,0.,-0.707106781186547));
#22888=CARTESIAN_POINT('',(0.841298510752802,-0.04763,-0.504455939115715));
#22889=CARTESIAN_POINT('Ctrl Pts',(0.841298510752802,-0.04763,-0.504455939115715));
#22890=CARTESIAN_POINT('Ctrl Pts',(0.838633903678357,-0.0740444353928835,
-0.508899795931835));
#22891=CARTESIAN_POINT('Ctrl Pts',(0.833661031856294,-0.0999305678883309,
-0.517157748491652));
#22892=CARTESIAN_POINT('Ctrl Pts',(0.820511285096538,-0.142345102874864,
-0.537715343527944));
#22893=CARTESIAN_POINT('Ctrl Pts',(0.813159949759,-0.159766064500479,-0.548874290046456));
#22894=CARTESIAN_POINT('Ctrl Pts',(0.795684265985088,-0.190326085855194,
-0.573915184558107));
#22895=CARTESIAN_POINT('Ctrl Pts',(0.78555112003688,-0.203463743702801,
-0.587792702767295));
#22896=CARTESIAN_POINT('Ctrl Pts',(0.763642258217233,-0.224161999508995,
-0.615966552324775));
#22897=CARTESIAN_POINT('Ctrl Pts',(0.750785745543687,-0.232861760990032,
-0.631684198665438));
#22898=CARTESIAN_POINT('Ctrl Pts',(0.722929908501543,-0.244251601209411,
-0.663382628119203));
#22899=CARTESIAN_POINT('Ctrl Pts',(0.707917883896095,-0.246942143572133,
-0.679352081686668));
#22900=CARTESIAN_POINT('Ctrl Pts',(0.679352081686668,-0.246942143572133,
-0.707917883896095));
#22901=CARTESIAN_POINT('Ctrl Pts',(0.663382628119203,-0.244251601209411,
-0.722929908501543));
#22902=CARTESIAN_POINT('Ctrl Pts',(0.631684198665438,-0.232861760990032,
-0.750785745543687));
#22903=CARTESIAN_POINT('Ctrl Pts',(0.615966552324775,-0.224161999508995,
-0.763642258217232));
#22904=CARTESIAN_POINT('Ctrl Pts',(0.587792702767295,-0.203463743702801,
-0.78555112003688));
#22905=CARTESIAN_POINT('Ctrl Pts',(0.573915184558107,-0.190326085855194,
-0.795684265985088));
#22906=CARTESIAN_POINT('Ctrl Pts',(0.548874290046456,-0.159766064500479,
-0.813159949759));
#22907=CARTESIAN_POINT('Ctrl Pts',(0.537715343527944,-0.142345102874864,
-0.820511285096538));
#22908=CARTESIAN_POINT('Ctrl Pts',(0.517157748491652,-0.099930567888331,
-0.833661031856294));
#22909=CARTESIAN_POINT('Ctrl Pts',(0.508899795931835,-0.0740444353928835,
-0.838633903678357));
#22910=CARTESIAN_POINT('Ctrl Pts',(0.504455939115715,-0.04763,-0.841298510752801));
#22911=CARTESIAN_POINT('Origin',(0.707106781186548,-0.04763,-0.707106781186547));
#22912=CARTESIAN_POINT('Origin',(0.,-0.166705,0.));
#22913=CARTESIAN_POINT('',(-0.980948,-0.28578,1.20131482833E-16));
#22914=CARTESIAN_POINT('Origin',(0.,-0.28578,0.));
#22915=CARTESIAN_POINT('',(-0.980948,-0.166705,1.20131482833E-16));
#22916=CARTESIAN_POINT('',(0.951592097314,-0.04763,0.238183666596899));
#22917=CARTESIAN_POINT('Origin',(0.,-0.04763,0.));
#22918=CARTESIAN_POINT('',(0.951592097314,-0.04763,-0.238183666596899));
#22919=CARTESIAN_POINT('Ctrl Pts',(0.951592097314,-0.04763,0.238183666596899));
#22920=CARTESIAN_POINT('Ctrl Pts',(0.952850216871763,-0.0740444353928835,
0.233157223576062));
#22921=CARTESIAN_POINT('Ctrl Pts',(0.955173119738174,-0.099930567888331,
0.223801617934945));
#22922=CARTESIAN_POINT('Ctrl Pts',(0.960411259488514,-0.142345102874864,
0.199966927975188));
#22923=CARTESIAN_POINT('Ctrl Pts',(0.963103647174702,-0.15976606450048,
0.1868781821531));
#22924=CARTESIAN_POINT('Ctrl Pts',(0.968453058988463,-0.190326085855194,
0.15681442133453));
#22925=CARTESIAN_POINT('Ctrl Pts',(0.971100730005489,-0.203463743702801,
0.139836317888042));
#22926=CARTESIAN_POINT('Ctrl Pts',(0.975530745318961,-0.224161999508995,
0.104422493053067));
#22927=CARTESIAN_POINT('Ctrl Pts',(0.977553872336861,-0.232861760990032,
0.0842175114474172));
#22928=CARTESIAN_POINT('Ctrl Pts',(0.980270995488453,-0.244251601209411,
0.0421062857595697));
#22929=CARTESIAN_POINT('Ctrl Pts',(0.980948,-0.246942143572133,0.0201990724523194));
#22930=CARTESIAN_POINT('Ctrl Pts',(0.980948,-0.246942143572133,-0.0201990724523194));
#22931=CARTESIAN_POINT('Ctrl Pts',(0.980270995488453,-0.244251601209411,
-0.0421062857595697));
#22932=CARTESIAN_POINT('Ctrl Pts',(0.977553872336861,-0.232861760990032,
-0.0842175114474172));
#22933=CARTESIAN_POINT('Ctrl Pts',(0.975530745318961,-0.224161999508995,
-0.104422493053067));
#22934=CARTESIAN_POINT('Ctrl Pts',(0.971100730005489,-0.203463743702801,
-0.139836317888042));
#22935=CARTESIAN_POINT('Ctrl Pts',(0.968453058988463,-0.190326085855194,
-0.15681442133453));
#22936=CARTESIAN_POINT('Ctrl Pts',(0.963103647174702,-0.15976606450048,
-0.1868781821531));
#22937=CARTESIAN_POINT('Ctrl Pts',(0.960411259488514,-0.142345102874864,
-0.199966927975188));
#22938=CARTESIAN_POINT('Ctrl Pts',(0.955173119738174,-0.099930567888331,
-0.223801617934945));
#22939=CARTESIAN_POINT('Ctrl Pts',(0.952850216871763,-0.0740444353928835,
-0.233157223576062));
#22940=CARTESIAN_POINT('Ctrl Pts',(0.951592097314,-0.0476299999999999,-0.238183666596899));
#22941=CARTESIAN_POINT('Origin',(0.,-0.04763,0.));
#22942=CARTESIAN_POINT('Origin',(0.,-0.04763,0.));
#22943=CARTESIAN_POINT('Origin',(1.,-0.04763,0.));
#22944=CARTESIAN_POINT('Origin',(1.,0.,0.));
#22945=CARTESIAN_POINT('Origin',(1.,-0.04763,0.));
#22946=CARTESIAN_POINT('Origin',(0.,-0.28578,0.));
#22947=CARTESIAN_POINT('Origin',(0.,-0.04763,0.));
#22948=CARTESIAN_POINT('',(0.,0.,0.));
#22949=CARTESIAN_POINT('Origin',(1.013815,0.445,0.));
#22950=CARTESIAN_POINT('',(-1.013815,0.445,-1.24156529467757E-16));
#22951=CARTESIAN_POINT('Origin',(0.,0.445,0.));
#22952=CARTESIAN_POINT('',(-0.991185,0.445,-1.21385153761287E-16));
#22953=CARTESIAN_POINT('Origin',(0.,0.445,0.));
#22954=CARTESIAN_POINT('Origin',(0.,0.4075,0.));
#22955=CARTESIAN_POINT('',(-1.013815,0.37,-1.24156529467757E-16));
#22956=CARTESIAN_POINT('Origin',(0.,0.37,0.));
#22957=CARTESIAN_POINT('',(-1.013815,0.4075,-1.24156529467757E-16));
#22958=CARTESIAN_POINT('Origin',(0.991185,0.37,0.));
#22959=CARTESIAN_POINT('',(-0.991185,0.37,-1.21385153761287E-16));
#22960=CARTESIAN_POINT('Origin',(0.,0.37,0.));
#22961=CARTESIAN_POINT('Origin',(0.,0.4075,0.));
#22962=CARTESIAN_POINT('',(-0.991185,0.4075,-1.21385153761287E-16));
#22963=CARTESIAN_POINT('Origin',(1.013815,-0.37,0.));
#22964=CARTESIAN_POINT('',(-1.013815,-0.37,-1.24156529467757E-16));
#22965=CARTESIAN_POINT('Origin',(0.,-0.37,0.));
#22966=CARTESIAN_POINT('',(-0.991185,-0.37,-1.21385153761287E-16));
#22967=CARTESIAN_POINT('Origin',(0.,-0.37,0.));
#22968=CARTESIAN_POINT('Origin',(0.,-0.4075,0.));
#22969=CARTESIAN_POINT('',(-1.013815,-0.445,-1.24156529467757E-16));
#22970=CARTESIAN_POINT('Origin',(0.,-0.445,0.));
#22971=CARTESIAN_POINT('',(-1.013815,-0.4075,-1.24156529467757E-16));
#22972=CARTESIAN_POINT('Origin',(0.991185,-0.445,0.));
#22973=CARTESIAN_POINT('',(-0.991185,-0.445,-1.21385153761287E-16));
#22974=CARTESIAN_POINT('Origin',(0.,-0.445,0.));
#22975=CARTESIAN_POINT('Origin',(0.,-0.4075,0.));
#22976=CARTESIAN_POINT('',(-0.991185,-0.4075,-1.21385153761287E-16));
#22977=CARTESIAN_POINT('',(0.,0.,0.));
#22978=CARTESIAN_POINT('',(0.,0.,0.));
#22979=CARTESIAN_POINT('',(0.,0.,0.));
#22980=CARTESIAN_POINT('',(0.,0.,0.));
#22981=CARTESIAN_POINT('',(0.,0.,0.));
#22982=CARTESIAN_POINT('',(0.,0.,0.));
#22983=CARTESIAN_POINT('Origin',(0.0866025403784439,-0.4,-0.15));
#22984=CARTESIAN_POINT('',(0.173205080756888,-0.4,0.));
#22985=CARTESIAN_POINT('',(0.0866025403784439,-0.4,-0.15));
#22986=CARTESIAN_POINT('',(0.173205080756888,-0.4,0.));
#22987=CARTESIAN_POINT('',(0.0866025403784439,-0.64,-0.15));
#22988=CARTESIAN_POINT('',(0.0866025403784439,-0.4,-0.15));
#22989=CARTESIAN_POINT('',(0.173205080756888,-0.64,0.));
#22990=CARTESIAN_POINT('',(0.173205080756888,-0.64,0.));
#22991=CARTESIAN_POINT('',(0.173205080756888,-0.4,0.));
#22992=CARTESIAN_POINT('Origin',(-0.0866025403784438,-0.4,-0.15));
#22993=CARTESIAN_POINT('',(-0.0866025403784438,-0.4,-0.15));
#22994=CARTESIAN_POINT('',(0.0866025403784439,-0.4,-0.15));
#22995=CARTESIAN_POINT('',(-0.0866025403784438,-0.64,-0.15));
#22996=CARTESIAN_POINT('',(-0.0866025403784438,-0.4,-0.15));
#22997=CARTESIAN_POINT('',(0.0866025403784439,-0.64,-0.15));
#22998=CARTESIAN_POINT('Origin',(-0.173205080756888,-0.4,-2.77555756156289E-17));
#22999=CARTESIAN_POINT('',(-0.173205080756888,-0.4,-2.12115047744981E-17));
#23000=CARTESIAN_POINT('',(-0.0866025403784438,-0.4,-0.15));
#23001=CARTESIAN_POINT('',(-0.173205080756888,-0.64,-2.77555756156289E-17));
#23002=CARTESIAN_POINT('',(-0.173205080756888,-0.4,-2.12115047744981E-17));
#23003=CARTESIAN_POINT('',(-0.0866025403784438,-0.64,-0.15));
#23004=CARTESIAN_POINT('Origin',(-0.0866025403784439,-0.4,0.15));
#23005=CARTESIAN_POINT('',(-0.0866025403784439,-0.4,0.15));
#23006=CARTESIAN_POINT('',(-0.173205080756888,-0.4,-2.12115047744981E-17));
#23007=CARTESIAN_POINT('',(-0.0866025403784439,-0.64,0.15));
#23008=CARTESIAN_POINT('',(-0.0866025403784439,-0.4,0.15));
#23009=CARTESIAN_POINT('',(-0.173205080756888,-0.64,-2.12115047744981E-17));
#23010=CARTESIAN_POINT('Origin',(0.0866025403784439,-0.4,0.15));
#23011=CARTESIAN_POINT('',(0.0866025403784439,-0.4,0.15));
#23012=CARTESIAN_POINT('',(-0.0866025403784439,-0.4,0.15));
#23013=CARTESIAN_POINT('',(0.0866025403784439,-0.64,0.15));
#23014=CARTESIAN_POINT('',(0.0866025403784439,-0.4,0.15));
#23015=CARTESIAN_POINT('',(-0.0866025403784439,-0.64,0.15));
#23016=CARTESIAN_POINT('Origin',(0.173205080756888,-0.4,0.));
#23017=CARTESIAN_POINT('',(0.0866025403784439,-0.4,0.15));
#23018=CARTESIAN_POINT('',(0.0866025403784439,-0.64,0.15));
#23019=CARTESIAN_POINT('Origin',(0.,-0.4,-2.77555756156289E-17));
#23020=CARTESIAN_POINT('Origin',(0.,-0.64,-2.77555756156289E-17));
#23021=CARTESIAN_POINT('Origin',(0.,-1.6,0.));
#23022=CARTESIAN_POINT('',(-0.2,-1.6,2.44929359829471E-17));
#23023=CARTESIAN_POINT('Origin',(0.,-1.6,0.));
#23024=CARTESIAN_POINT('',(-0.16,-1.6,-1.95943487863577E-17));
#23025=CARTESIAN_POINT('Origin',(0.,-1.6,0.));
#23026=CARTESIAN_POINT('Origin',(0.,-3.,0.));
#23027=CARTESIAN_POINT('',(-0.2,-3.,2.44929359829471E-17));
#23028=CARTESIAN_POINT('',(-0.2,-3.,2.44929359829471E-17));
#23029=CARTESIAN_POINT('Origin',(0.,-3.,0.));
#23030=CARTESIAN_POINT('Origin',(0.,-3.,0.));
#23031=CARTESIAN_POINT('Origin',(0.3,0.4,0.));
#23032=CARTESIAN_POINT('',(-0.3,0.4,-3.67394039744206E-17));
#23033=CARTESIAN_POINT('Origin',(0.,0.4,0.));
#23034=CARTESIAN_POINT('Origin',(0.,0.375,0.));
#23035=CARTESIAN_POINT('',(-0.35,0.35,-4.28626379701573E-17));
#23036=CARTESIAN_POINT('Origin',(0.,0.35,0.));
#23037=CARTESIAN_POINT('',(-0.325,0.375,-3.9801020972289E-17));
#23038=CARTESIAN_POINT('Origin',(0.,0.19,0.));
#23039=CARTESIAN_POINT('',(-0.35,0.03,-4.28626379701574E-17));
#23040=CARTESIAN_POINT('Origin',(0.,0.03,0.));
#23041=CARTESIAN_POINT('',(-0.35,0.19,-4.28626379701574E-17));
#23042=CARTESIAN_POINT('Origin',(0.,0.0149999999999999,0.));
#23043=CARTESIAN_POINT('',(-0.32,-3.29597460435593E-17,-3.91886975727153E-17));
#23044=CARTESIAN_POINT('Origin',(0.,0.,0.));
#23045=CARTESIAN_POINT('',(-0.335,0.0149999999999999,-4.10256677714363E-17));
#23046=CARTESIAN_POINT('Origin',(0.22,0.,0.));
#23047=CARTESIAN_POINT('',(-0.22,-6.93889390390723E-18,-2.69422295812418E-17));
#23048=CARTESIAN_POINT('Origin',(0.,0.,0.));
#23049=CARTESIAN_POINT('Origin',(0.,-0.02,0.));
#23050=CARTESIAN_POINT('',(-0.1954,-0.0492,2.39295984553393E-17));
#23051=CARTESIAN_POINT('Origin',(0.,-0.0492,0.));
#23052=CARTESIAN_POINT('',(-0.21,-0.02,-2.57175827820944E-17));
#23053=CARTESIAN_POINT('Origin',(0.,-0.8,0.));
#23054=CARTESIAN_POINT('',(-0.1954,-1.5646,2.39295984553393E-17));
#23055=CARTESIAN_POINT('Origin',(0.,-1.5646,0.));
#23056=CARTESIAN_POINT('',(-0.1954,-0.8,-2.39295984553393E-17));
#23057=CARTESIAN_POINT('Origin',(0.,-1.58,0.));
#23058=CARTESIAN_POINT('',(-0.18,-1.58,-2.20436423846524E-17));
#23059=CARTESIAN_POINT('',(0.,0.,0.));
#23060=CARTESIAN_POINT('',(0.,0.,0.));
#23061=CARTESIAN_POINT('Origin',(0.,0.,0.));
#23062=CARTESIAN_POINT('',(-1.070235,-0.308121667383195,-1.31065986708547E-16));
#23063=CARTESIAN_POINT('',(-1.31065986708547E-16,-0.308121667383195,1.070235));
#23064=CARTESIAN_POINT('Origin',(0.,-0.308121667383195,0.));
#23065=CARTESIAN_POINT('Origin',(0.,-0.308121667383195,0.));
#23066=CARTESIAN_POINT('',(-1.31065986708547E-16,0.308121667383195,1.070235));
#23067=CARTESIAN_POINT('Origin',(-1.34711147906209E-16,0.,1.1));
#23068=CARTESIAN_POINT('',(-1.070235,0.308121667383195,1.31065986708547E-16));
#23069=CARTESIAN_POINT('Origin',(0.,0.308121667383195,0.));
#23070=CARTESIAN_POINT('Origin',(0.,0.308121667383195,0.));
#23071=CARTESIAN_POINT('Origin',(0.,0.,0.));
#23072=CARTESIAN_POINT('',(-1.070235,0.5,-1.31065986708547E-16));
#23073=CARTESIAN_POINT('',(-1.070235,0.,-1.31065986708547E-16));
#23074=CARTESIAN_POINT('Origin',(0.,0.5,0.));
#23075=CARTESIAN_POINT('Origin',(0.,0.,0.));
#23076=CARTESIAN_POINT('',(-0.6,-0.44,-7.34788079488412E-17));
#23077=CARTESIAN_POINT('Origin',(0.,-0.44,0.));
#23078=CARTESIAN_POINT('',(-0.6,0.44,-7.34788079488412E-17));
#23079=CARTESIAN_POINT('',(-0.6,0.,-7.34788079488412E-17));
#23080=CARTESIAN_POINT('Origin',(0.,0.44,0.));
#23081=CARTESIAN_POINT('Origin',(0.,0.47,0.));
#23082=CARTESIAN_POINT('',(-0.66,0.5,-8.08266887437253E-17));
#23083=CARTESIAN_POINT('',(-0.63,0.47,-7.71527483462832E-17));
#23084=CARTESIAN_POINT('Origin',(0.,0.5,0.));
#23085=CARTESIAN_POINT('Origin',(1.070235,0.5,0.));
#23086=CARTESIAN_POINT('Origin',(0.,0.,0.));
#23087=CARTESIAN_POINT('',(-1.070235,-0.5,-1.31065986708547E-16));
#23088=CARTESIAN_POINT('Origin',(0.,-0.5,0.));
#23089=CARTESIAN_POINT('',(-1.070235,0.,-1.31065986708547E-16));
#23090=CARTESIAN_POINT('Origin',(0.66,-0.5,0.));
#23091=CARTESIAN_POINT('',(-0.66,-0.5,-8.08266887437253E-17));
#23092=CARTESIAN_POINT('Origin',(0.,-0.5,0.));
#23093=CARTESIAN_POINT('Origin',(0.,-0.47,0.));
#23094=CARTESIAN_POINT('',(-0.63,-0.47,-7.71527483462832E-17));
#23095=CARTESIAN_POINT('',(0.,0.,0.));
#23096=CARTESIAN_POINT('Origin',(0.,0.,0.));
#23097=CARTESIAN_POINT('',(-1.129765,0.308121667383195,-1.38356309103871E-16));
#23098=CARTESIAN_POINT('',(-1.38356309103871E-16,0.308121667383195,1.129765));
#23099=CARTESIAN_POINT('Origin',(0.,0.308121667383195,0.));
#23100=CARTESIAN_POINT('Origin',(0.,0.308121667383195,0.));
#23101=CARTESIAN_POINT('',(-1.38356309103871E-16,-0.308121667383195,1.129765));
#23102=CARTESIAN_POINT('Origin',(-1.34711147906209E-16,0.,1.1));
#23103=CARTESIAN_POINT('',(-1.129765,-0.308121667383195,1.38356309103871E-16));
#23104=CARTESIAN_POINT('Origin',(0.,-0.308121667383195,0.));
#23105=CARTESIAN_POINT('Origin',(0.,-0.308121667383195,0.));
#23106=CARTESIAN_POINT('Origin',(0.,0.,0.));
#23107=CARTESIAN_POINT('',(-1.129765,-0.5,-1.38356309103871E-16));
#23108=CARTESIAN_POINT('Origin',(0.,-0.5,0.));
#23109=CARTESIAN_POINT('',(-1.129765,0.,-1.38356309103871E-16));
#23110=CARTESIAN_POINT('Origin',(1.54,0.5,0.));
#23111=CARTESIAN_POINT('',(-1.54,0.5,-1.88595607068692E-16));
#23112=CARTESIAN_POINT('Origin',(0.,0.5,0.));
#23113=CARTESIAN_POINT('',(-1.129765,0.5,-1.38356309103871E-16));
#23114=CARTESIAN_POINT('Origin',(0.,0.5,0.));
#23115=CARTESIAN_POINT('Origin',(0.,0.47,0.));
#23116=CARTESIAN_POINT('',(-1.6,0.44,-1.95943487863577E-16));
#23117=CARTESIAN_POINT('Origin',(0.,0.44,0.));
#23118=CARTESIAN_POINT('',(-1.57,0.47,-1.92269547466134E-16));
#23119=CARTESIAN_POINT('Origin',(0.,0.,0.));
#23120=CARTESIAN_POINT('',(-1.6,-0.44,-1.95943487863577E-16));
#23121=CARTESIAN_POINT('Origin',(0.,-0.44,0.));
#23122=CARTESIAN_POINT('',(-1.6,0.,-1.95943487863577E-16));
#23123=CARTESIAN_POINT('Origin',(0.,-0.47,0.));
#23124=CARTESIAN_POINT('',(-1.54,-0.5,-1.88595607068692E-16));
#23125=CARTESIAN_POINT('Origin',(0.,-0.5,0.));
#23126=CARTESIAN_POINT('',(-1.57,-0.47,-1.92269547466134E-16));
#23127=CARTESIAN_POINT('Origin',(1.129765,-0.5,0.));
#23128=CARTESIAN_POINT('Origin',(0.,0.,0.));
#23129=CARTESIAN_POINT('',(-1.129765,0.,-1.38356309103871E-16));
#23130=CARTESIAN_POINT('',(0.,0.,0.));
#23131=CARTESIAN_POINT('Origin',(1.1,0.,0.));
#23132=CARTESIAN_POINT('',(1.1,-2.23201749654651E-33,0.29765));
#23133=CARTESIAN_POINT('',(1.1,-2.23201749654651E-33,-0.29765));
#23134=CARTESIAN_POINT('Origin',(1.1,0.,0.));
#23135=CARTESIAN_POINT('Origin',(0.685838782044607,0.,-0.860014630714833));
#23136=CARTESIAN_POINT('',(0.918550922801216,-5.31350540756609E-33,-0.674432891191581));
#23137=CARTESIAN_POINT('',(0.453126641287998,8.49470414473068E-34,-1.04559637023808));
#23138=CARTESIAN_POINT('Origin',(0.685838782044607,0.,-0.860014630714833));
#23139=CARTESIAN_POINT('Origin',(-0.244773027351946,0.,-1.07242070340001));
#23140=CARTESIAN_POINT('',(0.0454142657089739,-2.23201749654651E-33,-1.1386540593921));
#23141=CARTESIAN_POINT('',(-0.534960320412865,-2.23201749654651E-33,-1.00618734740791));
#23142=CARTESIAN_POINT('Origin',(-0.244773027351946,0.,-1.07242070340001));
#23143=CARTESIAN_POINT('Origin',(-0.991065754692661,0.,-0.477272113029314));
#23144=CARTESIAN_POINT('',(-0.86192025974432,8.49470414473067E-34,-0.745445496560469));
#23145=CARTESIAN_POINT('',(-1.120211249641,-5.31350540756609E-33,-0.209098729498159));
#23146=CARTESIAN_POINT('Origin',(-0.991065754692661,0.,-0.477272113029314));
#23147=CARTESIAN_POINT('Origin',(-0.991065754692661,0.,0.477272113029314));
#23148=CARTESIAN_POINT('',(-1.120211249641,-2.23201749654651E-33,0.209098729498159));
#23149=CARTESIAN_POINT('',(-0.86192025974432,-2.23201749654651E-33,0.745445496560469));
#23150=CARTESIAN_POINT('Origin',(-0.991065754692661,0.,0.477272113029314));
#23151=CARTESIAN_POINT('Origin',(-0.244773027351946,0.,1.07242070340001));
#23152=CARTESIAN_POINT('',(-0.534960320412866,-2.23201749654651E-33,1.00618734740791));
#23153=CARTESIAN_POINT('',(0.0454142657089737,-2.23201749654651E-33,1.1386540593921));
#23154=CARTESIAN_POINT('Origin',(-0.244773027351946,0.,1.07242070340001));
#23155=CARTESIAN_POINT('Origin',(0.685838782044607,0.,0.860014630714833));
#23156=CARTESIAN_POINT('',(0.453126641287998,-2.23201749654651E-33,1.04559637023808));
#23157=CARTESIAN_POINT('',(0.918550922801216,-2.23201749654651E-33,0.674432891191581));
#23158=CARTESIAN_POINT('Origin',(0.685838782044607,0.,0.860014630714833));
#23159=CARTESIAN_POINT('',(0.,0.,0.));
#23160=CARTESIAN_POINT('Origin',(0.685838782044607,0.,0.860014630714833));
#23161=CARTESIAN_POINT('',(0.413083465285518,-0.05953,0.993751811093549));
#23162=CARTESIAN_POINT('',(0.876916659919095,-0.05953,0.623857181492959));
#23163=CARTESIAN_POINT('Ctrl Pts',(0.413083465285518,-0.05953,0.993751811093549));
#23164=CARTESIAN_POINT('Ctrl Pts',(0.419070565453383,-0.0925528133349865,
0.991263089003441));
#23165=CARTESIAN_POINT('Ctrl Pts',(0.430199341854858,-0.124911173756694,
0.986608710139579));
#23166=CARTESIAN_POINT('Ctrl Pts',(0.457978755888596,-0.177924977804098,
0.973971221090534));
#23167=CARTESIAN_POINT('Ctrl Pts',(0.473077587363685,-0.199697230012983,
0.966820759530997));
#23168=CARTESIAN_POINT('Ctrl Pts',(0.507057380724533,-0.237895043532788,
0.949440676105255));
#23169=CARTESIAN_POINT('Ctrl Pts',(0.525933334162555,-0.254319232363049,
0.939198248544428));
#23170=CARTESIAN_POINT('Ctrl Pts',(0.564362943424238,-0.28018331644634,
0.916597376014514));
#23171=CARTESIAN_POINT('Ctrl Pts',(0.585840553788742,-0.29104845371857,
0.903141581680914));
#23172=CARTESIAN_POINT('Ctrl Pts',(0.629305439856167,-0.30527573347708,
0.873412008702649));
#23173=CARTESIAN_POINT('Ctrl Pts',(0.651278921914856,-0.308638795020976,
0.857118508332695));
#23174=CARTESIAN_POINT('Ctrl Pts',(0.690705563850638,-0.308638795020976,
0.825676810575914));
#23175=CARTESIAN_POINT('Ctrl Pts',(0.711480111898423,-0.30527573347708,
0.807879894508811));
#23176=CARTESIAN_POINT('Ctrl Pts',(0.750136149454208,-0.29104845371857,
0.772120216227122));
#23177=CARTESIAN_POINT('Ctrl Pts',(0.768033796848072,-0.28018331644634,
0.754175290318038));
#23178=CARTESIAN_POINT('Ctrl Pts',(0.798619410861634,-0.254319232363049,
0.721738358858166));
#23179=CARTESIAN_POINT('Ctrl Pts',(0.812805334167529,-0.237895043532788,
0.705614819529209));
#23180=CARTESIAN_POINT('Ctrl Pts',(0.837310877969633,-0.199697230012983,
0.676354402927683));
#23181=CARTESIAN_POINT('Ctrl Pts',(0.847641868610495,-0.177924977804098,
0.663225258065736));
#23182=CARTESIAN_POINT('Ctrl Pts',(0.866144010579847,-0.124911173756694,
0.638954437806245));
#23183=CARTESIAN_POINT('Ctrl Pts',(0.873158080166742,-0.0925528133349865,
0.62914037979579));
#23184=CARTESIAN_POINT('Ctrl Pts',(0.876916659919095,-0.05953,0.623857181492959));
#23185=CARTESIAN_POINT('',(0.437601487681057,-0.05953,1.03511272300331));
#23186=CARTESIAN_POINT('Origin',(0.685838782044607,-0.05953,0.860014630714833));
#23187=CARTESIAN_POINT('',(0.911784794170997,-0.05953,0.656964154625313));
#23188=CARTESIAN_POINT('Ctrl Pts',(0.911784794170998,-0.0595300000000001,
0.656964154625312));
#23189=CARTESIAN_POINT('Ctrl Pts',(0.909827729890942,-0.0762225747374255,
0.659680317203144));
#23190=CARTESIAN_POINT('Ctrl Pts',(0.907004864562642,-0.0928409665394228,
0.663576540841106));
#23191=CARTESIAN_POINT('Ctrl Pts',(0.895234408667242,-0.144299303100741,
0.679480524217551));
#23192=CARTESIAN_POINT('Ctrl Pts',(0.882797231409153,-0.177024326825049,
0.695831250979106));
#23193=CARTESIAN_POINT('Ctrl Pts',(0.854332839576145,-0.227269801620064,
0.73042219438957));
#23194=CARTESIAN_POINT('Ctrl Pts',(0.834863020612702,-0.251265615809407,
0.752807465209441));
#23195=CARTESIAN_POINT('Ctrl Pts',(0.800439809856111,-0.279889827963178,
0.789147407129766));
#23196=CARTESIAN_POINT('Ctrl Pts',(0.781998747691871,-0.290879136862659,
0.80756613568454));
#23197=CARTESIAN_POINT('Ctrl Pts',(0.742239891936898,-0.305251990234487,
0.844254137480382));
#23198=CARTESIAN_POINT('Ctrl Pts',(0.720906778729541,-0.308638795020976,
0.862505527716294));
#23199=CARTESIAN_POINT('Ctrl Pts',(0.680463863683392,-0.308638795020976,
0.894757676234429));
#23200=CARTESIAN_POINT('Ctrl Pts',(0.657923009631182,-0.305251990234488,
0.91149460735272));
#23201=CARTESIAN_POINT('Ctrl Pts',(0.613307674922609,-0.290879136862659,
0.942092777160053));
#23202=CARTESIAN_POINT('Ctrl Pts',(0.591247219971725,-0.279889827963178,
0.955972930713954));
#23203=CARTESIAN_POINT('Ctrl Pts',(0.548158511259202,-0.251265615809407,
0.981446681891443));
#23204=CARTESIAN_POINT('Ctrl Pts',(0.522002043615455,-0.227269801620063,
0.995447160474328));
#23205=CARTESIAN_POINT('Ctrl Pts',(0.481944444320713,-0.177024326825049,
1.01550068154148));
#23206=CARTESIAN_POINT('Ctrl Pts',(0.463236132117164,-0.14429930310074,
1.0239876538093));
#23207=CARTESIAN_POINT('Ctrl Pts',(0.445111721969657,-0.0928409665394226,
1.03192403056628));
#23208=CARTESIAN_POINT('Ctrl Pts',(0.440685038163619,-0.0762225747374254,
1.03380912944435));
#23209=CARTESIAN_POINT('Ctrl Pts',(0.437601487681056,-0.05953,1.03511272300331));
#23210=CARTESIAN_POINT('Origin',(0.685838782044607,-0.05953,0.860014630714833));
#23211=CARTESIAN_POINT('Origin',(0.,-0.208355,0.));
#23212=CARTESIAN_POINT('',(0.0548532617164168,-0.05953,1.12247250791415));
#23213=CARTESIAN_POINT('Origin',(0.,-0.05953,0.));
#23214=CARTESIAN_POINT('',(-0.536443649899848,-0.05953,0.987512846410683));
#23215=CARTESIAN_POINT('Ctrl Pts',(0.0548532617164173,-0.0595300000000001,
1.12247250791414));
#23216=CARTESIAN_POINT('Ctrl Pts',(0.05150947068137,-0.0762225747374254,
1.12263591311425));
#23217=CARTESIAN_POINT('Ctrl Pts',(0.0467032526342597,-0.0928409665394227,
1.12285816383385));
#23218=CARTESIAN_POINT('Ctrl Pts',(0.0269302585198975,-0.144299303100741,
1.12357162229597));
#23219=CARTESIAN_POINT('Ctrl Pts',(0.006392292392153,-0.177024326825049,
1.12404235695137));
#23220=CARTESIAN_POINT('Ctrl Pts',(-0.0383992541984087,-0.227269801620063,
1.12335509974011));
#23221=CARTESIAN_POINT('Ctrl Pts',(-0.0680399972366993,-0.251265615809407,
1.12208997038458));
#23222=CARTESIAN_POINT('Ctrl Pts',(-0.117914228755037,-0.279889827963178,
1.1178344036749));
#23223=CARTESIAN_POINT('Ctrl Pts',(-0.14381238480104,-0.290879136862659,
1.11490049012186));
#23224=CARTESIAN_POINT('Ctrl Pts',(-0.19728546073067,-0.305251990234488,
1.10669035995599));
#23225=CARTESIAN_POINT('Ctrl Pts',(-0.224855950742601,-0.308638795020976,
1.10139101611326));
#23226=CARTESIAN_POINT('Ctrl Pts',(-0.275287440920027,-0.308638795020976,
1.0898803575765));
#23227=CARTESIAN_POINT('Ctrl Pts',(-0.302426893214945,-0.305251990234488,
1.08269251410343));
#23228=CARTESIAN_POINT('Ctrl Pts',(-0.35416671187353,-0.290879136862659,
1.06688848765783));
#23229=CARTESIAN_POINT('Ctrl Pts',(-0.3787731215897,-0.279889827963178,
1.05829506364875));
#23230=CARTESIAN_POINT('Ctrl Pts',(-0.425554672694338,-0.251265615809407,
1.04048957871266));
#23231=CARTESIAN_POINT('Ctrl Pts',(-0.452808978448581,-0.227269801620063,
1.02876878445619));
#23232=CARTESIAN_POINT('Ctrl Pts',(-0.493462957200432,-0.177024326825049,
1.0099536580922));
#23233=CARTESIAN_POINT('Ctrl Pts',(-0.511762781179148,-0.14429930310074,
1.00061845128527));
#23234=CARTESIAN_POINT('Ctrl Pts',(-0.529268075276157,-0.0928409665394226,
0.991396466802468));
#23235=CARTESIAN_POINT('Ctrl Pts',(-0.533501897135713,-0.0762225747374254,
0.989110885965947));
#23236=CARTESIAN_POINT('Ctrl Pts',(-0.536443649899848,-0.0595300000000001,
0.987512846410683));
#23237=CARTESIAN_POINT('',(-0.843383895613249,-0.05953,0.742736168477219));
#23238=CARTESIAN_POINT('Origin',(0.,-0.05953,0.));
#23239=CARTESIAN_POINT('',(-1.10653577764992,-0.05953,0.196295654879792));
#23240=CARTESIAN_POINT('Ctrl Pts',(-0.843383895613249,-0.0595300000000001,
0.742736168477219));
#23241=CARTESIAN_POINT('Ctrl Pts',(-0.84559647055299,-0.0762225747374255,
0.740223768851062));
#23242=CARTESIAN_POINT('Ctrl Pts',(-0.848766861100456,-0.0928409665394227,
0.736604687327351));
#23243=CARTESIAN_POINT('Ctrl Pts',(-0.861652925570091,-0.144299303100741,
0.721590372101268));
#23244=CARTESIAN_POINT('Ctrl Pts',(-0.87482617317514,-0.177024326825049,
0.705826641853758));
#23245=CARTESIAN_POINT('Ctrl Pts',(-0.902215926359523,-0.227269801620063,
0.670378702718353));
#23246=CARTESIAN_POINT('Ctrl Pts',(-0.919707509403859,-0.251265615809407,
0.646415841396062));
#23247=CARTESIAN_POINT('Ctrl Pts',(-0.947476448101718,-0.279889827963178,
0.604769294586516));
#23248=CARTESIAN_POINT('Ctrl Pts',(-0.961329858300736,-0.290879136862659,
0.582692035672022));
#23249=CARTESIAN_POINT('Ctrl Pts',(-0.988250837578047,-0.305251990234488,
0.535766169015486));
#23250=CARTESIAN_POINT('Ctrl Pts',(-1.00129756308006,-0.308638795020976,
0.510906605094603));
#23251=CARTESIAN_POINT('Ctrl Pts',(-1.02374168767024,-0.308638795020976,
0.46430090015576));
#23252=CARTESIAN_POINT('Ctrl Pts',(-1.03504317708586,-0.305251990234488,
0.438600874831839));
#23253=CARTESIAN_POINT('Ctrl Pts',(-1.05494634094458,-0.290879136862659,
0.388295406390235));
#23254=CARTESIAN_POINT('Ctrl Pts',(-1.06356957703048,-0.279889827963178,
0.363699428370917));
#23255=CARTESIAN_POINT('Ctrl Pts',(-1.0788165083757,-0.251265615809407,
0.316022600643821));
#23256=CARTESIAN_POINT('Ctrl Pts',(-1.08664560412098,-0.227269801620063,
0.287406530683752));
#23257=CARTESIAN_POINT('Ctrl Pts',(-1.09728268713976,-0.177024326825049,
0.243890930799337));
#23258=CARTESIAN_POINT('Ctrl Pts',(-1.10139388218929,-0.144299303100741,
0.22376314604679));
#23259=CARTESIAN_POINT('Ctrl Pts',(-1.10509821673782,-0.0928409665394227,
0.204327142733961));
#23260=CARTESIAN_POINT('Ctrl Pts',(-1.10595102243643,-0.0762225747374254,
0.199591971170104));
#23261=CARTESIAN_POINT('Ctrl Pts',(-1.10653577764992,-0.0595300000000001,
0.196295654879792));
#23262=CARTESIAN_POINT('',(-1.123812,-0.05953,1.37627276864339E-16));
#23263=CARTESIAN_POINT('Origin',(0.,-0.05953,0.));
#23264=CARTESIAN_POINT('',(-1.123812,-0.35718,1.37627276864339E-16));
#23265=CARTESIAN_POINT('',(-1.123812,-0.208355,1.37627276864339E-16));
#23266=CARTESIAN_POINT('Origin',(0.,-0.35718,0.));
#23267=CARTESIAN_POINT('',(-1.10653577764992,-0.05953,-0.196295654879793));
#23268=CARTESIAN_POINT('Origin',(0.,-0.05953,0.));
#23269=CARTESIAN_POINT('',(-0.843383895613249,-0.05953,-0.742736168477219));
#23270=CARTESIAN_POINT('Ctrl Pts',(-1.10653577764992,-0.0595300000000001,
-0.196295654879792));
#23271=CARTESIAN_POINT('Ctrl Pts',(-1.10595102243643,-0.0762225747374255,
-0.199591971170104));
#23272=CARTESIAN_POINT('Ctrl Pts',(-1.10509821673782,-0.0928409665394228,
-0.204327142733962));
#23273=CARTESIAN_POINT('Ctrl Pts',(-1.10139388218929,-0.144299303100741,
-0.22376314604679));
#23274=CARTESIAN_POINT('Ctrl Pts',(-1.09728268713976,-0.177024326825049,
-0.243890930799338));
#23275=CARTESIAN_POINT('Ctrl Pts',(-1.08664560412098,-0.227269801620063,
-0.287406530683753));
#23276=CARTESIAN_POINT('Ctrl Pts',(-1.0788165083757,-0.251265615809407,
-0.316022600643821));
#23277=CARTESIAN_POINT('Ctrl Pts',(-1.06356957703048,-0.279889827963178,
-0.363699428370918));
#23278=CARTESIAN_POINT('Ctrl Pts',(-1.05494634094458,-0.290879136862659,
-0.388295406390235));
#23279=CARTESIAN_POINT('Ctrl Pts',(-1.03504317708586,-0.305251990234488,
-0.438600874831839));
#23280=CARTESIAN_POINT('Ctrl Pts',(-1.02374168767024,-0.308638795020976,
-0.46430090015576));
#23281=CARTESIAN_POINT('Ctrl Pts',(-1.00129756308006,-0.308638795020976,
-0.510906605094603));
#23282=CARTESIAN_POINT('Ctrl Pts',(-0.988250837578047,-0.305251990234488,
-0.535766169015486));
#23283=CARTESIAN_POINT('Ctrl Pts',(-0.961329858300736,-0.290879136862659,
-0.582692035672022));
#23284=CARTESIAN_POINT('Ctrl Pts',(-0.947476448101718,-0.279889827963178,
-0.604769294586516));
#23285=CARTESIAN_POINT('Ctrl Pts',(-0.919707509403859,-0.251265615809407,
-0.646415841396062));
#23286=CARTESIAN_POINT('Ctrl Pts',(-0.902215926359523,-0.227269801620064,
-0.670378702718353));
#23287=CARTESIAN_POINT('Ctrl Pts',(-0.87482617317514,-0.177024326825049,
-0.705826641853758));
#23288=CARTESIAN_POINT('Ctrl Pts',(-0.861652925570091,-0.144299303100741,
-0.721590372101268));
#23289=CARTESIAN_POINT('Ctrl Pts',(-0.848766861100456,-0.0928409665394229,
-0.736604687327351));
#23290=CARTESIAN_POINT('Ctrl Pts',(-0.84559647055299,-0.0762225747374255,
-0.740223768851063));
#23291=CARTESIAN_POINT('Ctrl Pts',(-0.843383895613249,-0.0595300000000001,
-0.742736168477219));
#23292=CARTESIAN_POINT('',(-0.536443649899847,-0.05953,-0.987512846410683));
#23293=CARTESIAN_POINT('Origin',(0.,-0.05953,0.));
#23294=CARTESIAN_POINT('',(0.0548532617164172,-0.05953,-1.12247250791415));
#23295=CARTESIAN_POINT('Ctrl Pts',(-0.536443649899848,-0.0595300000000001,
-0.987512846410683));
#23296=CARTESIAN_POINT('Ctrl Pts',(-0.533501897135712,-0.0762225747374254,
-0.989110885965947));
#23297=CARTESIAN_POINT('Ctrl Pts',(-0.529268075276156,-0.0928409665394227,
-0.991396466802469));
#23298=CARTESIAN_POINT('Ctrl Pts',(-0.511762781179147,-0.144299303100741,
-1.00061845128527));
#23299=CARTESIAN_POINT('Ctrl Pts',(-0.493462957200432,-0.177024326825049,
-1.0099536580922));
#23300=CARTESIAN_POINT('Ctrl Pts',(-0.45280897844858,-0.227269801620063,
-1.02876878445619));
#23301=CARTESIAN_POINT('Ctrl Pts',(-0.425554672694337,-0.251265615809407,
-1.04048957871266));
#23302=CARTESIAN_POINT('Ctrl Pts',(-0.3787731215897,-0.279889827963178,
-1.05829506364875));
#23303=CARTESIAN_POINT('Ctrl Pts',(-0.354166711873529,-0.290879136862659,
-1.06688848765783));
#23304=CARTESIAN_POINT('Ctrl Pts',(-0.302426893214944,-0.305251990234488,
-1.08269251410343));
#23305=CARTESIAN_POINT('Ctrl Pts',(-0.275287440920027,-0.308638795020976,
-1.0898803575765));
#23306=CARTESIAN_POINT('Ctrl Pts',(-0.224855950742601,-0.308638795020976,
-1.10139101611326));
#23307=CARTESIAN_POINT('Ctrl Pts',(-0.19728546073067,-0.305251990234488,
-1.10669035995599));
#23308=CARTESIAN_POINT('Ctrl Pts',(-0.143812384801039,-0.290879136862659,
-1.11490049012186));
#23309=CARTESIAN_POINT('Ctrl Pts',(-0.117914228755037,-0.279889827963178,
-1.1178344036749));
#23310=CARTESIAN_POINT('Ctrl Pts',(-0.0680399972366989,-0.251265615809407,
-1.12208997038458));
#23311=CARTESIAN_POINT('Ctrl Pts',(-0.0383992541984084,-0.227269801620063,
-1.12335509974011));
#23312=CARTESIAN_POINT('Ctrl Pts',(0.00639229239215326,-0.177024326825049,
-1.12404235695137));
#23313=CARTESIAN_POINT('Ctrl Pts',(0.0269302585198977,-0.144299303100741,
-1.12357162229597));
#23314=CARTESIAN_POINT('Ctrl Pts',(0.04670325263426,-0.0928409665394228,
-1.12285816383385));
#23315=CARTESIAN_POINT('Ctrl Pts',(0.0515094706813703,-0.0762225747374255,
-1.12263591311425));
#23316=CARTESIAN_POINT('Ctrl Pts',(0.0548532617164176,-0.0595300000000001,
-1.12247250791414));
#23317=CARTESIAN_POINT('',(0.437601487681057,-0.05953,-1.03511272300331));
#23318=CARTESIAN_POINT('Origin',(0.,-0.05953,0.));
#23319=CARTESIAN_POINT('',(0.911784794170997,-0.05953,-0.656964154625313));
#23320=CARTESIAN_POINT('Ctrl Pts',(0.437601487681056,-0.0595300000000001,
-1.03511272300331));
#23321=CARTESIAN_POINT('Ctrl Pts',(0.440685038163619,-0.0762225747374255,
-1.03380912944435));
#23322=CARTESIAN_POINT('Ctrl Pts',(0.445111721969657,-0.0928409665394228,
-1.03192403056628));
#23323=CARTESIAN_POINT('Ctrl Pts',(0.463236132117164,-0.144299303100741,
-1.0239876538093));
#23324=CARTESIAN_POINT('Ctrl Pts',(0.481944444320713,-0.177024326825049,
-1.01550068154148));
#23325=CARTESIAN_POINT('Ctrl Pts',(0.522002043615455,-0.227269801620064,
-0.995447160474328));
#23326=CARTESIAN_POINT('Ctrl Pts',(0.548158511259203,-0.251265615809407,
-0.981446681891443));
#23327=CARTESIAN_POINT('Ctrl Pts',(0.591247219971725,-0.279889827963178,
-0.955972930713954));
#23328=CARTESIAN_POINT('Ctrl Pts',(0.613307674922609,-0.290879136862659,
-0.942092777160053));
#23329=CARTESIAN_POINT('Ctrl Pts',(0.657923009631182,-0.305251990234487,
-0.91149460735272));
#23330=CARTESIAN_POINT('Ctrl Pts',(0.680463863683393,-0.308638795020976,
-0.894757676234429));
#23331=CARTESIAN_POINT('Ctrl Pts',(0.720906778729542,-0.308638795020976,
-0.862505527716294));
#23332=CARTESIAN_POINT('Ctrl Pts',(0.742239891936899,-0.305251990234488,
-0.844254137480381));
#23333=CARTESIAN_POINT('Ctrl Pts',(0.781998747691872,-0.290879136862659,
-0.80756613568454));
#23334=CARTESIAN_POINT('Ctrl Pts',(0.800439809856112,-0.279889827963178,
-0.789147407129765));
#23335=CARTESIAN_POINT('Ctrl Pts',(0.834863020612702,-0.251265615809407,
-0.752807465209441));
#23336=CARTESIAN_POINT('Ctrl Pts',(0.854332839576145,-0.227269801620064,
-0.73042219438957));
#23337=CARTESIAN_POINT('Ctrl Pts',(0.882797231409153,-0.177024326825049,
-0.695831250979106));
#23338=CARTESIAN_POINT('Ctrl Pts',(0.895234408667242,-0.144299303100741,
-0.679480524217551));
#23339=CARTESIAN_POINT('Ctrl Pts',(0.907004864562642,-0.0928409665394228,
-0.663576540841106));
#23340=CARTESIAN_POINT('Ctrl Pts',(0.909827729890942,-0.0762225747374256,
-0.659680317203144));
#23341=CARTESIAN_POINT('Ctrl Pts',(0.911784794170998,-0.0595300000000001,
-0.656964154625312));
#23342=CARTESIAN_POINT('',(1.08212377959455,-0.05953,-0.303251606722892));
#23343=CARTESIAN_POINT('Origin',(0.,-0.05953,0.));
#23344=CARTESIAN_POINT('',(1.08212377959455,-0.05953,0.303251606722892));
#23345=CARTESIAN_POINT('Ctrl Pts',(1.08212377959455,-0.0595300000000001,
-0.303251606722892));
#23346=CARTESIAN_POINT('Ctrl Pts',(1.0830271513892,-0.0762225747374255,
-0.300028012588062));
#23347=CARTESIAN_POINT('Ctrl Pts',(1.08431331394788,-0.0928409665394228,
-0.2953917518996));
#23348=CARTESIAN_POINT('Ctrl Pts',(1.08940878963422,-0.144299303100741,
-0.276273267473431));
#23349=CARTESIAN_POINT('Ctrl Pts',(1.09443784939331,-0.177024326825049,
-0.256354979351213));
#23350=CARTESIAN_POINT('Ctrl Pts',(1.10373487993589,-0.227269801620064,
-0.212533521233765));
#23351=CARTESIAN_POINT('Ctrl Pts',(1.10909715583869,-0.251265615809407,
-0.183354415742157));
#23352=CARTESIAN_POINT('Ctrl Pts',(1.1160463456491,-0.279889827963178,-0.133783682657561));
#23353=CARTESIAN_POINT('Ctrl Pts',(1.11894887330541,-0.290879136862659,
-0.107881990270302));
#23354=CARTESIAN_POINT('Ctrl Pts',(1.12284346704144,-0.305251990234488,
-0.0539226701638766));
#23355=CARTESIAN_POINT('Ctrl Pts',(1.123812,-0.308638795020976,-0.025864214957475));
#23356=CARTESIAN_POINT('Ctrl Pts',(1.123812,-0.308638795020976,0.025864214957475));
#23357=CARTESIAN_POINT('Ctrl Pts',(1.12284346704144,-0.305251990234488,
0.0539226701638766));
#23358=CARTESIAN_POINT('Ctrl Pts',(1.11894887330541,-0.290879136862659,
0.107881990270302));
#23359=CARTESIAN_POINT('Ctrl Pts',(1.1160463456491,-0.279889827963178,0.133783682657561));
#23360=CARTESIAN_POINT('Ctrl Pts',(1.10909715583869,-0.251265615809407,
0.183354415742157));
#23361=CARTESIAN_POINT('Ctrl Pts',(1.10373487993589,-0.227269801620064,
0.212533521233765));
#23362=CARTESIAN_POINT('Ctrl Pts',(1.09443784939331,-0.177024326825049,
0.256354979351213));
#23363=CARTESIAN_POINT('Ctrl Pts',(1.08940878963422,-0.144299303100741,
0.276273267473431));
#23364=CARTESIAN_POINT('Ctrl Pts',(1.08431331394788,-0.0928409665394228,
0.2953917518996));
#23365=CARTESIAN_POINT('Ctrl Pts',(1.0830271513892,-0.0762225747374255,
0.300028012588062));
#23366=CARTESIAN_POINT('Ctrl Pts',(1.08212377959455,-0.0595300000000001,
0.303251606722892));
#23367=CARTESIAN_POINT('Origin',(0.,-0.05953,0.));
#23368=CARTESIAN_POINT('Origin',(0.,-0.05953,0.));
#23369=CARTESIAN_POINT('',(0.0589974094846122,-0.05953,1.07456964270265));
#23370=CARTESIAN_POINT('Origin',(0.,-0.05953,0.));
#23371=CARTESIAN_POINT('Origin',(-0.244773027351946,-0.05953,1.07242070340001));
#23372=CARTESIAN_POINT('Origin',(-0.244773027351946,0.,1.07242070340001));
#23373=CARTESIAN_POINT('',(-0.519393123750572,-0.05953,0.942555777842682));
#23374=CARTESIAN_POINT('Ctrl Pts',(-0.519393123750572,-0.05953,0.942555777842682));
#23375=CARTESIAN_POINT('Ctrl Pts',(-0.513714466572041,-0.0925528133349865,
0.945684988399766));
#23376=CARTESIAN_POINT('Ctrl Pts',(-0.503136848051455,-0.124911173756694,
0.951483858396181));
#23377=CARTESIAN_POINT('Ctrl Pts',(-0.47593627990192,-0.177924977804098,
0.965323333309091));
#23378=CARTESIAN_POINT('Ctrl Pts',(-0.460931856495794,-0.199697230012983,
0.972669835243841));
#23379=CARTESIAN_POINT('Ctrl Pts',(-0.426157505475872,-0.237895043532788,
0.988400002689705));
#23380=CARTESIAN_POINT('Ctrl Pts',(-0.406380688682952,-0.254319232363049,
0.996771768218699));
#23381=CARTESIAN_POINT('Ctrl Pts',(-0.364750145543744,-0.28018331644634,
1.01272583306292));
#23382=CARTESIAN_POINT('Ctrl Pts',(-0.340838910881557,-0.29104845371857,
1.02112815447116));
#23383=CARTESIAN_POINT('Ctrl Pts',(-0.290495481564827,-0.30527573347708,
1.036574285215));
#23384=CARTESIAN_POINT('Ctrl Pts',(-0.264056468041074,-0.308638795020976,
1.04359501395068));
#23385=CARTESIAN_POINT('Ctrl Pts',(-0.214892249704082,-0.308638795020976,
1.05481642595959));
#23386=CARTESIAN_POINT('Ctrl Pts',(-0.188025341585962,-0.30527573347708,
1.05996242598502));
#23387=CARTESIAN_POINT('Ctrl Pts',(-0.135965654106109,-0.29104845371857,
1.06788913840721));
#23388=CARTESIAN_POINT('Ctrl Pts',(-0.110776745452494,-0.28018331644634,
1.07069360430242));
#23389=CARTESIAN_POINT('Ctrl Pts',(-0.0663467128214646,-0.254319232363049,
1.07438230428002));
#23390=CARTESIAN_POINT('Ctrl Pts',(-0.0448960436540983,-0.237895043532788,
1.07542044338697));
#23391=CARTESIAN_POINT('Ctrl Pts',(-0.00674037211528124,-0.199697230012983,
1.07633607767727));
#23392=CARTESIAN_POINT('Ctrl Pts',(0.00996567398334777,-0.177924977804098,
1.07622728347683));
#23393=CARTESIAN_POINT('Ctrl Pts',(0.0404772621979741,-0.124911173756694,
1.07556023164702));
#23394=CARTESIAN_POINT('Ctrl Pts',(0.0525234025782719,-0.0925528133349865,
1.07492508698591));
#23395=CARTESIAN_POINT('Ctrl Pts',(0.0589974094846124,-0.05953,1.07456964270265));
#23396=CARTESIAN_POINT('Origin',(-0.244773027351946,-0.05953,1.07242070340001));
#23397=CARTESIAN_POINT('Origin',(0.,-0.05953,0.));
#23398=CARTESIAN_POINT('',(-0.803348093619616,-0.05953,0.716109245731214));
#23399=CARTESIAN_POINT('Origin',(0.,-0.05953,0.));
#23400=CARTESIAN_POINT('Origin',(-0.991065754692661,-0.05953,0.477272113029314));
#23401=CARTESIAN_POINT('Origin',(-0.991065754692661,0.,0.477272113029314));
#23402=CARTESIAN_POINT('',(-1.06075609691358,-0.05953,0.181596019242328));
#23403=CARTESIAN_POINT('Ctrl Pts',(-1.06075609691358,-0.05953,0.181596019242328));
#23404=CARTESIAN_POINT('Ctrl Pts',(-1.05966202740332,-0.0925528133349865,
0.187986803072856));
#23405=CARTESIAN_POINT('Ctrl Pts',(-1.05760072925372,-0.124911173756694,
0.199872254546857));
#23406=CARTESIAN_POINT('Ctrl Pts',(-1.05146158959546,-0.177924977804098,
0.22976728653846));
#23407=CARTESIAN_POINT('Ctrl Pts',(-1.04785021111757,-0.199697230012983,
0.246078686169301));
#23408=CARTESIAN_POINT('Ctrl Pts',(-1.03846709802406,-0.237895043532788,
0.283073967563097));
#23409=CARTESIAN_POINT('Ctrl Pts',(-1.03268176429485,-0.254319232363049,
0.303755815985685));
#23410=CARTESIAN_POINT('Ctrl Pts',(-1.01919893537026,-0.28018331644634,
0.346251081972725));
#23411=CARTESIAN_POINT('Ctrl Pts',(-1.01085972381132,-0.29104845371857,
0.370184399726282));
#23412=CARTESIAN_POINT('Ctrl Pts',(-0.99154738033959,-0.30527573347708,
0.419174982698463));
#23413=CARTESIAN_POINT('Ctrl Pts',(-0.980551951791748,-0.308638795020976,
0.444223188605045));
#23414=CARTESIAN_POINT('Ctrl Pts',(-0.958671816228589,-0.308638795020976,
0.489657758261848));
#23415=CARTESIAN_POINT('Ctrl Pts',(-0.945943877838127,-0.30527573347708,
0.51387163140139));
#23416=CARTESIAN_POINT('Ctrl Pts',(-0.91968254693063,-0.29104845371857,
0.559515758398093));
#23417=CARTESIAN_POINT('Ctrl Pts',(-0.906170138993533,-0.28018331644634,
0.580957796077825));
#23418=CARTESIAN_POINT('Ctrl Pts',(-0.8813524085237,-0.254319232363049,
0.617994461173994));
#23419=CARTESIAN_POINT('Ctrl Pts',(-0.868789784891799,-0.237895043532788,
0.635412538795143));
#23420=CARTESIAN_POINT('Ctrl Pts',(-0.845715984518854,-0.199697230012983,
0.66581473268113));
#23421=CARTESIAN_POINT('Ctrl Pts',(-0.835214876415962,-0.177924977804098,
0.678808213394124));
#23422=CARTESIAN_POINT('Ctrl Pts',(-0.815669690204649,-0.124911173756694,
0.702247233627224));
#23423=CARTESIAN_POINT('Ctrl Pts',(-0.807662468433796,-0.0925528133349865,
0.711269279199861));
#23424=CARTESIAN_POINT('Ctrl Pts',(-0.803348093619616,-0.05953,0.716109245731214));
#23425=CARTESIAN_POINT('Origin',(-0.991065754692661,-0.05953,0.477272113029314));
#23426=CARTESIAN_POINT('Origin',(0.,-0.05953,0.));
#23427=CARTESIAN_POINT('',(-1.076188,-0.05953,1.31795018948079E-16));
#23428=CARTESIAN_POINT('Origin',(0.,-0.05953,0.));
#23429=CARTESIAN_POINT('',(-1.06075609691358,-0.05953,-0.181596019242328));
#23430=CARTESIAN_POINT('Origin',(0.,-0.05953,0.));
#23431=CARTESIAN_POINT('Origin',(-0.991065754692661,-0.05953,-0.477272113029314));
#23432=CARTESIAN_POINT('Origin',(-0.991065754692661,0.,-0.477272113029314));
#23433=CARTESIAN_POINT('',(-0.803348093619616,-0.05953,-0.716109245731215));
#23434=CARTESIAN_POINT('Ctrl Pts',(-0.803348093619616,-0.05953,-0.716109245731215));
#23435=CARTESIAN_POINT('Ctrl Pts',(-0.807662468433795,-0.0925528133349865,
-0.711269279199862));
#23436=CARTESIAN_POINT('Ctrl Pts',(-0.815669690204649,-0.124911173756694,
-0.702247233627224));
#23437=CARTESIAN_POINT('Ctrl Pts',(-0.835214876415962,-0.177924977804098,
-0.678808213394124));
#23438=CARTESIAN_POINT('Ctrl Pts',(-0.845715984518854,-0.199697230012983,
-0.66581473268113));
#23439=CARTESIAN_POINT('Ctrl Pts',(-0.868789784891799,-0.237895043532788,
-0.635412538795143));
#23440=CARTESIAN_POINT('Ctrl Pts',(-0.8813524085237,-0.254319232363049,
-0.617994461173994));
#23441=CARTESIAN_POINT('Ctrl Pts',(-0.906170138993533,-0.28018331644634,
-0.580957796077826));
#23442=CARTESIAN_POINT('Ctrl Pts',(-0.91968254693063,-0.29104845371857,
-0.559515758398093));
#23443=CARTESIAN_POINT('Ctrl Pts',(-0.945943877838127,-0.30527573347708,
-0.51387163140139));
#23444=CARTESIAN_POINT('Ctrl Pts',(-0.958671816228589,-0.308638795020976,
-0.489657758261848));
#23445=CARTESIAN_POINT('Ctrl Pts',(-0.980551951791748,-0.308638795020976,
-0.444223188605045));
#23446=CARTESIAN_POINT('Ctrl Pts',(-0.99154738033959,-0.30527573347708,
-0.419174982698463));
#23447=CARTESIAN_POINT('Ctrl Pts',(-1.01085972381132,-0.29104845371857,
-0.370184399726282));
#23448=CARTESIAN_POINT('Ctrl Pts',(-1.01919893537026,-0.28018331644634,
-0.346251081972725));
#23449=CARTESIAN_POINT('Ctrl Pts',(-1.03268176429485,-0.254319232363049,
-0.303755815985685));
#23450=CARTESIAN_POINT('Ctrl Pts',(-1.03846709802406,-0.237895043532788,
-0.283073967563097));
#23451=CARTESIAN_POINT('Ctrl Pts',(-1.04785021111757,-0.199697230012983,
-0.246078686169302));
#23452=CARTESIAN_POINT('Ctrl Pts',(-1.05146158959546,-0.177924977804098,
-0.229767286538461));
#23453=CARTESIAN_POINT('Ctrl Pts',(-1.05760072925372,-0.124911173756694,
-0.199872254546858));
#23454=CARTESIAN_POINT('Ctrl Pts',(-1.05966202740332,-0.0925528133349864,
-0.187986803072857));
#23455=CARTESIAN_POINT('Ctrl Pts',(-1.06075609691358,-0.05953,-0.181596019242328));
#23456=CARTESIAN_POINT('Origin',(-0.991065754692661,-0.05953,-0.477272113029314));
#23457=CARTESIAN_POINT('Origin',(0.,-0.05953,0.));
#23458=CARTESIAN_POINT('',(-0.519393123750572,-0.05953,-0.942555777842682));
#23459=CARTESIAN_POINT('Origin',(0.,-0.05953,0.));
#23460=CARTESIAN_POINT('Origin',(-0.244773027351946,-0.05953,-1.07242070340001));
#23461=CARTESIAN_POINT('Origin',(-0.244773027351946,0.,-1.07242070340001));
#23462=CARTESIAN_POINT('',(0.0589974094846125,-0.05953,-1.07456964270265));
#23463=CARTESIAN_POINT('Ctrl Pts',(0.0589974094846127,-0.05953,-1.07456964270265));
#23464=CARTESIAN_POINT('Ctrl Pts',(0.0525234025782722,-0.0925528133349865,
-1.07492508698591));
#23465=CARTESIAN_POINT('Ctrl Pts',(0.0404772621979744,-0.124911173756694,
-1.07556023164702));
#23466=CARTESIAN_POINT('Ctrl Pts',(0.0099656739833481,-0.177924977804098,
-1.07622728347683));
#23467=CARTESIAN_POINT('Ctrl Pts',(-0.00674037211528096,-0.199697230012983,
-1.07633607767727));
#23468=CARTESIAN_POINT('Ctrl Pts',(-0.044896043654098,-0.237895043532788,
-1.07542044338697));
#23469=CARTESIAN_POINT('Ctrl Pts',(-0.0663467128214644,-0.254319232363049,
-1.07438230428002));
#23470=CARTESIAN_POINT('Ctrl Pts',(-0.110776745452493,-0.28018331644634,
-1.07069360430242));
#23471=CARTESIAN_POINT('Ctrl Pts',(-0.135965654106109,-0.29104845371857,
-1.06788913840721));
#23472=CARTESIAN_POINT('Ctrl Pts',(-0.188025341585962,-0.30527573347708,
-1.05996242598502));
#23473=CARTESIAN_POINT('Ctrl Pts',(-0.214892249704082,-0.308638795020976,
-1.05481642595959));
#23474=CARTESIAN_POINT('Ctrl Pts',(-0.264056468041074,-0.308638795020976,
-1.04359501395068));
#23475=CARTESIAN_POINT('Ctrl Pts',(-0.290495481564827,-0.30527573347708,
-1.036574285215));
#23476=CARTESIAN_POINT('Ctrl Pts',(-0.340838910881557,-0.291048453718569,
-1.02112815447116));
#23477=CARTESIAN_POINT('Ctrl Pts',(-0.364750145543744,-0.28018331644634,
-1.01272583306292));
#23478=CARTESIAN_POINT('Ctrl Pts',(-0.406380688682952,-0.254319232363049,
-0.996771768218699));
#23479=CARTESIAN_POINT('Ctrl Pts',(-0.426157505475872,-0.237895043532788,
-0.988400002689705));
#23480=CARTESIAN_POINT('Ctrl Pts',(-0.460931856495794,-0.199697230012983,
-0.972669835243841));
#23481=CARTESIAN_POINT('Ctrl Pts',(-0.475936279901919,-0.177924977804098,
-0.965323333309091));
#23482=CARTESIAN_POINT('Ctrl Pts',(-0.503136848051454,-0.124911173756694,
-0.951483858396181));
#23483=CARTESIAN_POINT('Ctrl Pts',(-0.513714466572041,-0.0925528133349865,
-0.945684988399766));
#23484=CARTESIAN_POINT('Ctrl Pts',(-0.519393123750572,-0.05953,-0.942555777842682));
#23485=CARTESIAN_POINT('Origin',(-0.244773027351946,-0.05953,-1.07242070340001));
#23486=CARTESIAN_POINT('Origin',(0.,-0.05953,0.));
#23487=CARTESIAN_POINT('',(0.413083465285518,-0.05953,-0.993751811093549));
#23488=CARTESIAN_POINT('Origin',(0.,-0.05953,0.));
#23489=CARTESIAN_POINT('Origin',(0.685838782044607,-0.05953,-0.860014630714833));
#23490=CARTESIAN_POINT('Origin',(0.685838782044607,0.,-0.860014630714833));
#23491=CARTESIAN_POINT('',(0.876916659919095,-0.05953,-0.623857181492959));
#23492=CARTESIAN_POINT('Ctrl Pts',(0.876916659919095,-0.05953,-0.623857181492958));
#23493=CARTESIAN_POINT('Ctrl Pts',(0.873158080166742,-0.0925528133349865,
-0.62914037979579));
#23494=CARTESIAN_POINT('Ctrl Pts',(0.866144010579847,-0.124911173756694,
-0.638954437806245));
#23495=CARTESIAN_POINT('Ctrl Pts',(0.847641868610495,-0.177924977804098,
-0.663225258065736));
#23496=CARTESIAN_POINT('Ctrl Pts',(0.837310877969633,-0.199697230012983,
-0.676354402927683));
#23497=CARTESIAN_POINT('Ctrl Pts',(0.81280533416753,-0.237895043532788,
-0.705614819529209));
#23498=CARTESIAN_POINT('Ctrl Pts',(0.798619410861634,-0.254319232363049,
-0.721738358858166));
#23499=CARTESIAN_POINT('Ctrl Pts',(0.768033796848072,-0.28018331644634,
-0.754175290318038));
#23500=CARTESIAN_POINT('Ctrl Pts',(0.750136149454208,-0.29104845371857,
-0.772120216227122));
#23501=CARTESIAN_POINT('Ctrl Pts',(0.711480111898423,-0.30527573347708,
-0.807879894508811));
#23502=CARTESIAN_POINT('Ctrl Pts',(0.690705563850638,-0.308638795020976,
-0.825676810575913));
#23503=CARTESIAN_POINT('Ctrl Pts',(0.651278921914856,-0.308638795020976,
-0.857118508332695));
#23504=CARTESIAN_POINT('Ctrl Pts',(0.629305439856167,-0.30527573347708,
-0.873412008702649));
#23505=CARTESIAN_POINT('Ctrl Pts',(0.585840553788742,-0.29104845371857,
-0.903141581680914));
#23506=CARTESIAN_POINT('Ctrl Pts',(0.564362943424239,-0.28018331644634,
-0.916597376014514));
#23507=CARTESIAN_POINT('Ctrl Pts',(0.525933334162556,-0.254319232363049,
-0.939198248544427));
#23508=CARTESIAN_POINT('Ctrl Pts',(0.507057380724533,-0.237895043532788,
-0.949440676105255));
#23509=CARTESIAN_POINT('Ctrl Pts',(0.473077587363686,-0.199697230012983,
-0.966820759530997));
#23510=CARTESIAN_POINT('Ctrl Pts',(0.457978755888596,-0.177924977804098,
-0.973971221090534));
#23511=CARTESIAN_POINT('Ctrl Pts',(0.430199341854858,-0.124911173756694,
-0.986608710139579));
#23512=CARTESIAN_POINT('Ctrl Pts',(0.419070565453384,-0.0925528133349865,
-0.991263089003441));
#23513=CARTESIAN_POINT('Ctrl Pts',(0.413083465285518,-0.05953,-0.993751811093549));
#23514=CARTESIAN_POINT('Origin',(0.685838782044607,-0.05953,-0.860014630714833));
#23515=CARTESIAN_POINT('Origin',(0.,-0.208355,0.));
#23516=CARTESIAN_POINT('',(-1.076188,-0.35718,1.31795018948079E-16));
#23517=CARTESIAN_POINT('Origin',(0.,-0.35718,0.));
#23518=CARTESIAN_POINT('',(-1.076188,-0.208355,1.31795018948079E-16));
#23519=CARTESIAN_POINT('',(1.03449977959455,-0.05953,0.296632461748266));
#23520=CARTESIAN_POINT('Origin',(0.,-0.05953,0.));
#23521=CARTESIAN_POINT('',(1.03449977959455,-0.05953,-0.296632461748266));
#23522=CARTESIAN_POINT('Ctrl Pts',(1.03449977959455,-0.05953,0.296632461748267));
#23523=CARTESIAN_POINT('Ctrl Pts',(1.03628691421076,-0.0925528133349865,
0.290399865505497));
#23524=CARTESIAN_POINT('Ctrl Pts',(1.03958665287714,-0.124911173756694,
0.278797079997872));
#23525=CARTESIAN_POINT('Ctrl Pts',(1.0470264474309,-0.177924977804098,0.249198913998601));
#23526=CARTESIAN_POINT('Ctrl Pts',(1.05084995891418,-0.199697230012983,
0.232935932341942));
#23527=CARTESIAN_POINT('Ctrl Pts',(1.05844771715377,-0.237895043532788,
0.195533155353269));
#23528=CARTESIAN_POINT('Ctrl Pts',(1.06220882929878,-0.254319232363049,
0.17438929156337));
#23529=CARTESIAN_POINT('Ctrl Pts',(1.06849922508772,-0.28018331644634,0.130252399648131));
#23530=CARTESIAN_POINT('Ctrl Pts',(1.07137013248666,-0.29104845371857,0.105070977154072));
#23531=CARTESIAN_POINT('Ctrl Pts',(1.07522652957392,-0.30527573347708,0.0525526752791107));
#23532=CARTESIAN_POINT('Ctrl Pts',(1.076188,-0.308638795020976,0.025214283908933));
#23533=CARTESIAN_POINT('Ctrl Pts',(1.076188,-0.308638795020976,-0.025214283908933));
#23534=CARTESIAN_POINT('Ctrl Pts',(1.07522652957392,-0.30527573347708,-0.0525526752791107));
#23535=CARTESIAN_POINT('Ctrl Pts',(1.07137013248666,-0.29104845371857,-0.105070977154072));
#23536=CARTESIAN_POINT('Ctrl Pts',(1.06849922508772,-0.28018331644634,-0.130252399648131));
#23537=CARTESIAN_POINT('Ctrl Pts',(1.06220882929878,-0.254319232363049,
-0.17438929156337));
#23538=CARTESIAN_POINT('Ctrl Pts',(1.05844771715377,-0.237895043532788,
-0.195533155353269));
#23539=CARTESIAN_POINT('Ctrl Pts',(1.05084995891418,-0.199697230012983,
-0.232935932341942));
#23540=CARTESIAN_POINT('Ctrl Pts',(1.0470264474309,-0.177924977804098,-0.249198913998601));
#23541=CARTESIAN_POINT('Ctrl Pts',(1.03958665287714,-0.124911173756694,
-0.278797079997872));
#23542=CARTESIAN_POINT('Ctrl Pts',(1.03628691421076,-0.0925528133349865,
-0.290399865505497));
#23543=CARTESIAN_POINT('Ctrl Pts',(1.03449977959455,-0.05953,-0.296632461748267));
#23544=CARTESIAN_POINT('Origin',(0.,-0.05953,0.));
#23545=CARTESIAN_POINT('Origin',(0.,-0.05953,0.));
#23546=CARTESIAN_POINT('Origin',(1.1,-0.05953,0.));
#23547=CARTESIAN_POINT('Origin',(1.1,0.,0.));
#23548=CARTESIAN_POINT('Origin',(1.1,-0.05953,0.));
#23549=CARTESIAN_POINT('Origin',(0.,-0.35718,0.));
#23550=CARTESIAN_POINT('Origin',(0.,-0.05953,0.));
#23551=CARTESIAN_POINT('',(0.,0.,0.));
#23552=CARTESIAN_POINT('Origin',(1.119765,0.495,0.));
#23553=CARTESIAN_POINT('',(-1.119765,0.495,-1.37131662304724E-16));
#23554=CARTESIAN_POINT('Origin',(0.,0.495,0.));
#23555=CARTESIAN_POINT('',(-1.085235,0.495,-1.32902956907268E-16));
#23556=CARTESIAN_POINT('Origin',(0.,0.495,0.));
#23557=CARTESIAN_POINT('Origin',(0.,0.4575,0.));
#23558=CARTESIAN_POINT('',(-1.119765,0.42,-1.37131662304724E-16));
#23559=CARTESIAN_POINT('Origin',(0.,0.42,0.));
#23560=CARTESIAN_POINT('',(-1.119765,0.4575,-1.37131662304724E-16));
#23561=CARTESIAN_POINT('Origin',(1.085235,0.42,0.));
#23562=CARTESIAN_POINT('',(-1.085235,0.42,-1.32902956907268E-16));
#23563=CARTESIAN_POINT('Origin',(0.,0.42,0.));
#23564=CARTESIAN_POINT('Origin',(0.,0.4575,0.));
#23565=CARTESIAN_POINT('',(-1.085235,0.4575,-1.32902956907268E-16));
#23566=CARTESIAN_POINT('Origin',(1.119765,-0.42,0.));
#23567=CARTESIAN_POINT('',(-1.119765,-0.42,-1.37131662304724E-16));
#23568=CARTESIAN_POINT('Origin',(0.,-0.42,0.));
#23569=CARTESIAN_POINT('',(-1.085235,-0.42,-1.32902956907268E-16));
#23570=CARTESIAN_POINT('Origin',(0.,-0.42,0.));
#23571=CARTESIAN_POINT('Origin',(0.,-0.4575,0.));
#23572=CARTESIAN_POINT('',(-1.119765,-0.495,-1.37131662304724E-16));
#23573=CARTESIAN_POINT('Origin',(0.,-0.495,0.));
#23574=CARTESIAN_POINT('',(-1.119765,-0.4575,-1.37131662304724E-16));
#23575=CARTESIAN_POINT('Origin',(1.085235,-0.495,0.));
#23576=CARTESIAN_POINT('',(-1.085235,-0.495,-1.32902956907268E-16));
#23577=CARTESIAN_POINT('Origin',(0.,-0.495,0.));
#23578=CARTESIAN_POINT('Origin',(0.,-0.4575,0.));
#23579=CARTESIAN_POINT('',(-1.085235,-0.4575,-1.32902956907268E-16));
#23580=CARTESIAN_POINT('',(0.,0.,0.));
#23581=CARTESIAN_POINT('',(0.,0.,0.));
#23582=CARTESIAN_POINT('',(0.,0.,0.));
#23583=CARTESIAN_POINT('',(0.,0.,0.));
#23584=CARTESIAN_POINT('',(0.,0.,0.));
#23585=CARTESIAN_POINT('',(0.,0.,0.));
#23586=CARTESIAN_POINT('Origin',(0.375,0.5,0.));
#23587=CARTESIAN_POINT('',(-0.375,0.5,-4.59242549680257E-17));
#23588=CARTESIAN_POINT('Origin',(0.,0.5,0.));
#23589=CARTESIAN_POINT('Origin',(0.,0.475,0.));
#23590=CARTESIAN_POINT('',(-0.425,0.45,-5.20474889637625E-17));
#23591=CARTESIAN_POINT('Origin',(0.,0.45,0.));
#23592=CARTESIAN_POINT('',(-0.4,0.475,-4.89858719658941E-17));
#23593=CARTESIAN_POINT('Origin',(0.,0.24,0.));
#23594=CARTESIAN_POINT('',(-0.425,0.0299999999999998,-5.20474889637625E-17));
#23595=CARTESIAN_POINT('Origin',(0.,0.0299999999999998,0.));
#23596=CARTESIAN_POINT('',(-0.425,0.24,-5.20474889637625E-17));
#23597=CARTESIAN_POINT('Origin',(0.,0.0150000000000001,0.));
#23598=CARTESIAN_POINT('',(-0.395,4.85722573273506E-17,-4.83735485663204E-17));
#23599=CARTESIAN_POINT('Origin',(0.,0.,0.));
#23600=CARTESIAN_POINT('',(-0.41,0.0150000000000001,-5.02105187650415E-17));
#23601=CARTESIAN_POINT('Origin',(0.27,0.,0.));
#23602=CARTESIAN_POINT('',(-0.27,0.,-3.30654635769785E-17));
#23603=CARTESIAN_POINT('Origin',(0.,0.,0.));
#23604=CARTESIAN_POINT('Origin',(0.,-0.02,0.));
#23605=CARTESIAN_POINT('',(-0.24505,-0.0498999999999999,3.00099698131059E-17));
#23606=CARTESIAN_POINT('Origin',(0.,-0.0498999999999999,0.));
#23607=CARTESIAN_POINT('',(-0.26,-0.02,-3.18408167778312E-17));
#23608=CARTESIAN_POINT('Origin',(0.,-0.995,0.));
#23609=CARTESIAN_POINT('',(-0.24505,-1.95495,3.00099698131059E-17));
#23610=CARTESIAN_POINT('Origin',(0.,-1.95495,0.));
#23611=CARTESIAN_POINT('',(-0.24505,-0.995,-3.00099698131059E-17));
#23612=CARTESIAN_POINT('Origin',(0.,-1.975,0.));
#23613=CARTESIAN_POINT('',(-0.2,-2.,-2.44929359829471E-17));
#23614=CARTESIAN_POINT('Origin',(0.,-2.,0.));
#23615=CARTESIAN_POINT('',(-0.225,-1.975,-2.75545529808154E-17));
#23616=CARTESIAN_POINT('Origin',(0.,-2.,0.));
#23617=CARTESIAN_POINT('Origin',(0.115470053837925,-0.5,-0.2));
#23618=CARTESIAN_POINT('',(0.23094010767585,-0.5,0.));
#23619=CARTESIAN_POINT('',(0.115470053837925,-0.5,-0.2));
#23620=CARTESIAN_POINT('',(0.23094010767585,-0.5,0.));
#23621=CARTESIAN_POINT('',(0.115470053837925,-0.8,-0.2));
#23622=CARTESIAN_POINT('',(0.115470053837925,-0.5,-0.2));
#23623=CARTESIAN_POINT('',(0.23094010767585,-0.8,0.));
#23624=CARTESIAN_POINT('',(0.23094010767585,-0.8,0.));
#23625=CARTESIAN_POINT('',(0.23094010767585,-0.5,0.));
#23626=CARTESIAN_POINT('Origin',(-0.115470053837925,-0.5,-0.2));
#23627=CARTESIAN_POINT('',(-0.115470053837925,-0.5,-0.2));
#23628=CARTESIAN_POINT('',(0.115470053837925,-0.5,-0.2));
#23629=CARTESIAN_POINT('',(-0.115470053837925,-0.8,-0.2));
#23630=CARTESIAN_POINT('',(-0.115470053837925,-0.5,-0.2));
#23631=CARTESIAN_POINT('',(0.115470053837925,-0.8,-0.2));
#23632=CARTESIAN_POINT('Origin',(-0.23094010767585,-0.5,-2.77555756156289E-17));
#23633=CARTESIAN_POINT('',(-0.23094010767585,-0.5,-2.82820063659975E-17));
#23634=CARTESIAN_POINT('',(-0.115470053837925,-0.5,-0.2));
#23635=CARTESIAN_POINT('',(-0.23094010767585,-0.8,-2.77555756156289E-17));
#23636=CARTESIAN_POINT('',(-0.23094010767585,-0.5,-2.82820063659975E-17));
#23637=CARTESIAN_POINT('',(-0.115470053837925,-0.8,-0.2));
#23638=CARTESIAN_POINT('Origin',(-0.115470053837925,-0.5,0.2));
#23639=CARTESIAN_POINT('',(-0.115470053837925,-0.5,0.2));
#23640=CARTESIAN_POINT('',(-0.23094010767585,-0.5,-2.82820063659975E-17));
#23641=CARTESIAN_POINT('',(-0.115470053837925,-0.8,0.2));
#23642=CARTESIAN_POINT('',(-0.115470053837925,-0.5,0.2));
#23643=CARTESIAN_POINT('',(-0.23094010767585,-0.8,-2.82820063659975E-17));
#23644=CARTESIAN_POINT('Origin',(0.115470053837925,-0.5,0.2));
#23645=CARTESIAN_POINT('',(0.115470053837925,-0.5,0.2));
#23646=CARTESIAN_POINT('',(-0.115470053837925,-0.5,0.2));
#23647=CARTESIAN_POINT('',(0.115470053837925,-0.8,0.2));
#23648=CARTESIAN_POINT('',(0.115470053837925,-0.5,0.2));
#23649=CARTESIAN_POINT('',(-0.115470053837925,-0.8,0.2));
#23650=CARTESIAN_POINT('Origin',(0.23094010767585,-0.5,0.));
#23651=CARTESIAN_POINT('',(0.115470053837925,-0.5,0.2));
#23652=CARTESIAN_POINT('',(0.115470053837925,-0.8,0.2));
#23653=CARTESIAN_POINT('Origin',(0.,-0.5,0.));
#23654=CARTESIAN_POINT('Origin',(0.,-0.8,0.));
#23655=CARTESIAN_POINT('',(0.,0.,0.));
#23656=CARTESIAN_POINT('',(0.,0.,0.));
#23657=CARTESIAN_POINT('Origin',(0.,0.,0.));
#23658=CARTESIAN_POINT('',(-2.05,-1.65,2.51052593825207E-16));
#23659=CARTESIAN_POINT('Origin',(0.,-1.65,0.));
#23660=CARTESIAN_POINT('',(-2.05,-1.14891252930761,-2.51052593825207E-16));
#23661=CARTESIAN_POINT('',(-2.05,0.,2.51052593825207E-16));
#23662=CARTESIAN_POINT('Origin',(0.,-1.14891252930761,0.));
#23663=CARTESIAN_POINT('Origin',(0.,0.,0.));
#23664=CARTESIAN_POINT('',(-2.05,1.14891252930761,2.51052593825207E-16));
#23665=CARTESIAN_POINT('Origin',(0.,1.14891252930761,0.));
#23666=CARTESIAN_POINT('',(-2.05,1.65,-2.51052593825207E-16));
#23667=CARTESIAN_POINT('',(-2.05,0.,2.51052593825207E-16));
#23668=CARTESIAN_POINT('Origin',(0.,1.65,0.));
#23669=CARTESIAN_POINT('Origin',(0.,0.,0.));
#23670=CARTESIAN_POINT('',(-1.43895998899814E-16,-1.76221774462768E-32,
-2.35));
#23671=CARTESIAN_POINT('',(-1.43895998899814E-16,-1.76221774462768E-32,
2.35));
#23672=CARTESIAN_POINT('Origin',(0.,0.,0.));
#23673=CARTESIAN_POINT('Origin',(0.,1.55,-1.49));
#23674=CARTESIAN_POINT('',(-3.76384615384615,1.55,-2.13));
#23675=CARTESIAN_POINT('',(-1.81744325908679,1.55,-2.13));
#23676=CARTESIAN_POINT('',(0.,1.55,-2.13));
#23677=CARTESIAN_POINT('',(-2.46585583768694,1.55,-1.32648218523477));
#23678=CARTESIAN_POINT('',(-1.68,1.55,-0.84));
#23679=CARTESIAN_POINT('Origin',(0.,1.55,0.));
#23680=CARTESIAN_POINT('Origin',(0.,1.55,-1.49));
#23681=CARTESIAN_POINT('',(1.81744325908679,1.55,-2.13));
#23682=CARTESIAN_POINT('',(3.76384615384615,1.55,-2.13));
#23683=CARTESIAN_POINT('',(0.,1.55,-2.13));
#23684=CARTESIAN_POINT('',(2.46585583768694,1.55,-1.32648218523477));
#23685=CARTESIAN_POINT('Origin',(0.,1.55,0.));
#23686=CARTESIAN_POINT('',(3.78,1.55,-2.14));
#23687=CARTESIAN_POINT('Origin',(0.,-1.55,-1.49));
#23688=CARTESIAN_POINT('',(-1.81744325908679,-1.55,-2.13));
#23689=CARTESIAN_POINT('',(-3.76384615384615,-1.55,-2.13));
#23690=CARTESIAN_POINT('',(0.,-1.55,-2.13));
#23691=CARTESIAN_POINT('',(-2.46585583768694,-1.55,-1.32648218523477));
#23692=CARTESIAN_POINT('Origin',(0.,-1.55,0.));
#23693=CARTESIAN_POINT('',(-1.68,-1.55,-0.84));
#23694=CARTESIAN_POINT('Origin',(-3.78,0.,-2.14));
#23695=CARTESIAN_POINT('',(-3.76384615384615,0.,-2.13));
#23696=CARTESIAN_POINT('',(-2.46585583768694,0.,-1.32648218523477));
#23697=CARTESIAN_POINT('Origin',(0.,-1.55,-1.49));
#23698=CARTESIAN_POINT('',(3.76384615384615,-1.55,-2.13));
#23699=CARTESIAN_POINT('',(1.81744325908679,-1.55,-2.13));
#23700=CARTESIAN_POINT('',(0.,-1.55,-2.13));
#23701=CARTESIAN_POINT('',(2.46585583768694,-1.55,-1.32648218523477));
#23702=CARTESIAN_POINT('',(3.78,-1.55,-2.14));
#23703=CARTESIAN_POINT('Origin',(0.,-1.55,0.));
#23704=CARTESIAN_POINT('Origin',(1.68,0.,-0.84));
#23705=CARTESIAN_POINT('',(3.76384615384615,0.,-2.13));
#23706=CARTESIAN_POINT('',(2.46585583768694,0.,-1.32648218523477));
#23707=CARTESIAN_POINT('Origin',(0.,0.,-2.13));
#23708=CARTESIAN_POINT('',(-6.35,1.9,-2.13));
#23709=CARTESIAN_POINT('',(-6.35,-1.9,-2.13));
#23710=CARTESIAN_POINT('',(-6.35,1.9,-2.13));
#23711=CARTESIAN_POINT('',(6.35,-1.9,-2.13));
#23712=CARTESIAN_POINT('',(-6.35,-1.9,-2.13));
#23713=CARTESIAN_POINT('',(6.35,1.9,-2.13));
#23714=CARTESIAN_POINT('',(6.35,-1.9,-2.13));
#23715=CARTESIAN_POINT('',(6.35,1.9,-2.13));
#23716=CARTESIAN_POINT('',(4.1,7.9602041944578E-17,-2.13));
#23717=CARTESIAN_POINT('Origin',(4.75,0.,-2.13));
#23718=CARTESIAN_POINT('',(-5.4,7.9602041944578E-17,-2.13));
#23719=CARTESIAN_POINT('Origin',(-4.75,0.,-2.13));
#23720=CARTESIAN_POINT('',(1.81744325908679,-1.65,-2.13));
#23721=CARTESIAN_POINT('',(1.81744325908679,0.,-2.13));
#23722=CARTESIAN_POINT('',(-1.81744325908679,-1.65,-2.13));
#23723=CARTESIAN_POINT('',(0.,-1.65,-2.13));
#23724=CARTESIAN_POINT('',(-1.81744325908679,0.,-2.13));
#23725=CARTESIAN_POINT('',(-1.81744325908679,1.65,-2.13));
#23726=CARTESIAN_POINT('',(-1.81744325908679,0.,-2.13));
#23727=CARTESIAN_POINT('',(1.81744325908679,1.65,-2.13));
#23728=CARTESIAN_POINT('',(0.,1.65,-2.13));
#23729=CARTESIAN_POINT('',(1.81744325908679,0.,-2.13));
#23730=CARTESIAN_POINT('Origin',(0.,0.,0.));
#23731=CARTESIAN_POINT('Origin',(0.,1.65,0.));
#23732=CARTESIAN_POINT('Origin',(0.,-1.65,0.));
#23733=CARTESIAN_POINT('Origin',(0.,-1.65,0.));
#23734=CARTESIAN_POINT('Origin',(0.,1.65,0.));
#23735=CARTESIAN_POINT('Origin',(3.35,1.4,-3.33));
#23736=CARTESIAN_POINT('',(3.35,1.4,-3.33));
#23737=CARTESIAN_POINT('',(-3.35,1.4,-3.33));
#23738=CARTESIAN_POINT('',(1.675,1.4,-3.33));
#23739=CARTESIAN_POINT('',(3.35,1.4,-2.83));
#23740=CARTESIAN_POINT('',(3.35,1.4,-3.33));
#23741=CARTESIAN_POINT('',(-3.35,1.4,-2.83));
#23742=CARTESIAN_POINT('',(3.35,1.4,-2.83));
#23743=CARTESIAN_POINT('',(-3.35,1.4,-3.33));
#23744=CARTESIAN_POINT('Origin',(3.35,-1.4,-3.33));
#23745=CARTESIAN_POINT('',(3.35,-1.4,-3.33));
#23746=CARTESIAN_POINT('',(3.35,-0.7,-3.33));
#23747=CARTESIAN_POINT('',(3.35,-1.4,-2.83));
#23748=CARTESIAN_POINT('',(3.35,-1.4,-3.33));
#23749=CARTESIAN_POINT('',(3.35,-1.4,-2.83));
#23750=CARTESIAN_POINT('Origin',(-3.35,-1.4,-3.33));
#23751=CARTESIAN_POINT('',(-3.35,-1.4,-3.33));
#23752=CARTESIAN_POINT('',(-1.675,-1.4,-3.33));
#23753=CARTESIAN_POINT('',(-3.35,-1.4,-2.83));
#23754=CARTESIAN_POINT('',(-3.35,-1.4,-3.33));
#23755=CARTESIAN_POINT('',(-3.35,-1.4,-2.83));
#23756=CARTESIAN_POINT('Origin',(-3.35,1.4,-3.33));
#23757=CARTESIAN_POINT('',(-3.35,0.7,-3.33));
#23758=CARTESIAN_POINT('',(-3.35,1.4,-2.83));
#23759=CARTESIAN_POINT('Origin',(0.,0.,-2.83));
#23760=CARTESIAN_POINT('Origin',(-4.75,0.,-3.33));
#23761=CARTESIAN_POINT('',(-5.4,-7.9602041944578E-17,-3.33));
#23762=CARTESIAN_POINT('Origin',(-4.75,0.,-3.33));
#23763=CARTESIAN_POINT('',(-5.4,-7.9602041944578E-17,-3.33));
#23764=CARTESIAN_POINT('Origin',(4.75,0.,-3.33));
#23765=CARTESIAN_POINT('',(4.1,-7.9602041944578E-17,-3.33));
#23766=CARTESIAN_POINT('Origin',(4.75,0.,-3.33));
#23767=CARTESIAN_POINT('',(4.1,-7.9602041944578E-17,-3.33));
#23768=CARTESIAN_POINT('Origin',(6.35,1.9,-3.33));
#23769=CARTESIAN_POINT('',(6.35,1.9,-3.33));
#23770=CARTESIAN_POINT('',(-6.35,1.9,-3.33));
#23771=CARTESIAN_POINT('',(6.35,1.9,-3.33));
#23772=CARTESIAN_POINT('',(-6.35,1.9,-3.33));
#23773=CARTESIAN_POINT('',(6.35,1.9,-3.33));
#23774=CARTESIAN_POINT('Origin',(6.35,-1.9,-3.33));
#23775=CARTESIAN_POINT('',(6.35,-1.9,-3.33));
#23776=CARTESIAN_POINT('',(6.35,-1.9,-3.33));
#23777=CARTESIAN_POINT('',(6.35,-1.9,-3.33));
#23778=CARTESIAN_POINT('Origin',(-6.35,-1.9,-3.33));
#23779=CARTESIAN_POINT('',(-6.35,-1.9,-3.33));
#23780=CARTESIAN_POINT('',(-6.35,-1.9,-3.33));
#23781=CARTESIAN_POINT('',(-6.35,-1.9,-3.33));
#23782=CARTESIAN_POINT('Origin',(-6.35,1.9,-3.33));
#23783=CARTESIAN_POINT('',(-6.35,1.9,-3.33));
#23784=CARTESIAN_POINT('Origin',(0.,0.,-3.33));
#23785=CARTESIAN_POINT('',(0.,0.,0.));
#23786=CARTESIAN_POINT('Origin',(0.,0.,0.));
#23787=CARTESIAN_POINT('',(-1.8,-0.85,-2.20436423846524E-16));
#23788=CARTESIAN_POINT('Origin',(0.,-0.85,0.));
#23789=CARTESIAN_POINT('',(-1.8,0.85,-2.20436423846524E-16));
#23790=CARTESIAN_POINT('',(-1.8,0.,-2.20436423846524E-16));
#23791=CARTESIAN_POINT('Origin',(0.,0.85,0.));
#23792=CARTESIAN_POINT('Origin',(2.19089023002066,0.85,0.));
#23793=CARTESIAN_POINT('',(2.19089023002066,0.85,0.));
#23794=CARTESIAN_POINT('Origin',(0.,0.85,0.));
#23795=CARTESIAN_POINT('Origin',(3.99680288865056E-15,0.,0.));
#23796=CARTESIAN_POINT('',(3.85290688975075E-15,-1.76221774462768E-32,2.35));
#23797=CARTESIAN_POINT('',(3.85290688975075E-15,-1.76221774462768E-32,-2.35));
#23798=CARTESIAN_POINT('Origin',(3.99680288865056E-15,0.,0.));
#23799=CARTESIAN_POINT('',(2.19089023002066,-0.85,0.));
#23800=CARTESIAN_POINT('Origin',(0.,-0.85,0.));
#23801=CARTESIAN_POINT('Origin',(1.8,-0.85,0.));
#23802=CARTESIAN_POINT('Origin',(0.,1.55,0.));
#23803=CARTESIAN_POINT('',(1.42894191624432,1.8,0.825000000000001));
#23804=CARTESIAN_POINT('',(1.53744468918255,1.55,0.598968970568896));
#23805=CARTESIAN_POINT('Ctrl Pts',(1.42894191624432,1.8,0.825000000000001));
#23806=CARTESIAN_POINT('Ctrl Pts',(1.44466308895875,1.8,0.797770130104052));
#23807=CARTESIAN_POINT('Ctrl Pts',(1.46055812562105,1.79370633789704,0.768258557763732));
#23808=CARTESIAN_POINT('Ctrl Pts',(1.48824888379079,1.76817777258318,0.713138492740816));
#23809=CARTESIAN_POINT('Ctrl Pts',(1.50008999307766,1.74894552961493,0.687551581002689));
#23810=CARTESIAN_POINT('Ctrl Pts',(1.51812136280714,1.70460745840382,0.646764802471699));
#23811=CARTESIAN_POINT('Ctrl Pts',(1.52552758004446,1.67652816181843,0.628833667319578));
#23812=CARTESIAN_POINT('Ctrl Pts',(1.53516661651472,1.61494799959182,0.604921184808251));
#23813=CARTESIAN_POINT('Ctrl Pts',(1.53744468918255,1.58144291640553,0.598968970568896));
#23814=CARTESIAN_POINT('Ctrl Pts',(1.53744468918255,1.55,0.598968970568896));
#23815=CARTESIAN_POINT('',(1.42894191624432,1.3,0.825000000000001));
#23816=CARTESIAN_POINT('Ctrl Pts',(1.42894191624432,1.3,0.825000000000001));
#23817=CARTESIAN_POINT('Ctrl Pts',(1.4132207435299,1.3,0.852229869895949));
#23818=CARTESIAN_POINT('Ctrl Pts',(1.39561049050871,1.30629366210296,0.880751161609749));
#23819=CARTESIAN_POINT('Ctrl Pts',(1.36172049302549,1.33182222741682,0.932292094146256));
#23820=CARTESIAN_POINT('Ctrl Pts',(1.34548213209931,1.35105447038507,0.955340251466734));
#23821=CARTESIAN_POINT('Ctrl Pts',(1.31917543061769,1.39539254159618,0.99134926498299));
#23822=CARTESIAN_POINT('Ctrl Pts',(1.30734972067592,1.42347183818157,1.00672880483252));
#23823=CARTESIAN_POINT('Ctrl Pts',(1.29146042158868,1.48505200040818,1.02703269653942));
#23824=CARTESIAN_POINT('Ctrl Pts',(1.28744468918255,1.51855708359447,1.03198167246111));
#23825=CARTESIAN_POINT('Ctrl Pts',(1.28744468918255,1.58144291640553,1.03198167246111));
#23826=CARTESIAN_POINT('Ctrl Pts',(1.29146042158868,1.61494799959182,1.02703269653942));
#23827=CARTESIAN_POINT('Ctrl Pts',(1.30734972067592,1.67652816181843,1.00672880483252));
#23828=CARTESIAN_POINT('Ctrl Pts',(1.31917543061769,1.70460745840382,0.991349264982991));
#23829=CARTESIAN_POINT('Ctrl Pts',(1.34548213209931,1.74894552961493,0.955340251466735));
#23830=CARTESIAN_POINT('Ctrl Pts',(1.36172049302549,1.76817777258318,0.932292094146256));
#23831=CARTESIAN_POINT('Ctrl Pts',(1.39561049050871,1.79370633789704,0.880751161609749));
#23832=CARTESIAN_POINT('Ctrl Pts',(1.4132207435299,1.8,0.85222986989595));
#23833=CARTESIAN_POINT('Ctrl Pts',(1.42894191624432,1.8,0.825000000000001));
#23834=CARTESIAN_POINT('Ctrl Pts',(1.53744468918255,1.55,0.598968970568896));
#23835=CARTESIAN_POINT('Ctrl Pts',(1.53744468918255,1.51855708359447,0.598968970568896));
#23836=CARTESIAN_POINT('Ctrl Pts',(1.53516661651472,1.48505200040818,0.60492118480825));
#23837=CARTESIAN_POINT('Ctrl Pts',(1.52552758004446,1.42347183818157,0.628833667319578));
#23838=CARTESIAN_POINT('Ctrl Pts',(1.51812136280714,1.39539254159618,0.646764802471699));
#23839=CARTESIAN_POINT('Ctrl Pts',(1.50008999307766,1.35105447038507,0.687551581002689));
#23840=CARTESIAN_POINT('Ctrl Pts',(1.48824888379079,1.33182222741682,0.713138492740816));
#23841=CARTESIAN_POINT('Ctrl Pts',(1.46055812562105,1.30629366210296,0.768258557763732));
#23842=CARTESIAN_POINT('Ctrl Pts',(1.44466308895875,1.3,0.797770130104052));
#23843=CARTESIAN_POINT('Ctrl Pts',(1.42894191624432,1.3,0.825000000000001));
#23844=CARTESIAN_POINT('',(0.963525491562421,1.55,0.267616567329818));
#23845=CARTESIAN_POINT('',(0.125,1.55,-0.21650635094611));
#23846=CARTESIAN_POINT('Ctrl Pts',(0.963525491562421,1.55,0.267616567329818));
#23847=CARTESIAN_POINT('Ctrl Pts',(0.963525491562421,1.5815373526696,0.267616567329818));
#23848=CARTESIAN_POINT('Ctrl Pts',(0.961833761492987,1.61508042700263,0.273949373987484));
#23849=CARTESIAN_POINT('Ctrl Pts',(0.954308486908894,1.67663267125761,0.299111603474268));
#23850=CARTESIAN_POINT('Ctrl Pts',(0.948394987258249,1.70465411363682,0.31788699900678));
#23851=CARTESIAN_POINT('Ctrl Pts',(0.933155485613026,1.74889618382539,0.360174810895352));
#23852=CARTESIAN_POINT('Ctrl Pts',(0.92278792026947,1.76811531482682,0.386546956384144));
#23853=CARTESIAN_POINT('Ctrl Pts',(0.897143218189782,1.79367084275751,0.442820664919227));
#23854=CARTESIAN_POINT('Ctrl Pts',(0.881791875377343,1.8,0.472691670144998));
#23855=CARTESIAN_POINT('Ctrl Pts',(0.850258932191534,1.8,0.527308329855003));
#23856=CARTESIAN_POINT('Ctrl Pts',(0.832065554235658,1.79367084275751,0.555538485325664));
#23857=CARTESIAN_POINT('Ctrl Pts',(0.796153444118959,1.76811531482682,0.605884303066698));
#23858=CARTESIAN_POINT('Ctrl Pts',(0.778498278845144,1.74889618382539,0.62804895077401));
#23859=CARTESIAN_POINT('Ctrl Pts',(0.749495710301794,1.70465411363682,0.662390652284073));
#23860=CARTESIAN_POINT('Ctrl Pts',(0.73619249062986,1.67663267125761,0.676899590973058));
#23861=CARTESIAN_POINT('Ctrl Pts',(0.718163997970498,1.61508042700263,0.695997784676728));
#23862=CARTESIAN_POINT('Ctrl Pts',(0.713525491562421,1.5815373526696,0.700629269222037));
#23863=CARTESIAN_POINT('Ctrl Pts',(0.713525491562421,1.5184626473304,0.700629269222037));
#23864=CARTESIAN_POINT('Ctrl Pts',(0.718163997970498,1.48491957299737,0.695997784676728));
#23865=CARTESIAN_POINT('Ctrl Pts',(0.73619249062986,1.42336732874239,0.676899590973058));
#23866=CARTESIAN_POINT('Ctrl Pts',(0.749495710301794,1.39534588636318,0.662390652284073));
#23867=CARTESIAN_POINT('Ctrl Pts',(0.778498278845144,1.35110381617461,0.62804895077401));
#23868=CARTESIAN_POINT('Ctrl Pts',(0.796153444118959,1.33188468517318,0.605884303066698));
#23869=CARTESIAN_POINT('Ctrl Pts',(0.832065554235658,1.30632915724249,0.555538485325664));
#23870=CARTESIAN_POINT('Ctrl Pts',(0.850258932191534,1.3,0.527308329855003));
#23871=CARTESIAN_POINT('Ctrl Pts',(0.881791875377343,1.3,0.472691670144998));
#23872=CARTESIAN_POINT('Ctrl Pts',(0.897143218189782,1.30632915724249,0.442820664919227));
#23873=CARTESIAN_POINT('Ctrl Pts',(0.92278792026947,1.33188468517318,0.386546956384144));
#23874=CARTESIAN_POINT('Ctrl Pts',(0.933155485613026,1.35110381617461,0.360174810895352));
#23875=CARTESIAN_POINT('Ctrl Pts',(0.948394987258249,1.39534588636318,0.31788699900678));
#23876=CARTESIAN_POINT('Ctrl Pts',(0.954308486908894,1.42336732874239,0.299111603474268));
#23877=CARTESIAN_POINT('Ctrl Pts',(0.961833761492987,1.48491957299738,0.273949373987484));
#23878=CARTESIAN_POINT('Ctrl Pts',(0.963525491562421,1.5184626473304,0.267616567329818));
#23879=CARTESIAN_POINT('Ctrl Pts',(0.963525491562421,1.55,0.267616567329818));
#23880=CARTESIAN_POINT('Origin',(0.,1.55,0.));
#23881=CARTESIAN_POINT('',(-0.713525491562421,1.55,-0.700629269222037));
#23882=CARTESIAN_POINT('Ctrl Pts',(-0.713525491562421,1.55,-0.700629269222037));
#23883=CARTESIAN_POINT('Ctrl Pts',(-0.713525491562421,1.5184626473304,-0.700629269222037));
#23884=CARTESIAN_POINT('Ctrl Pts',(-0.718163997970498,1.48491957299737,
-0.695997784676728));
#23885=CARTESIAN_POINT('Ctrl Pts',(-0.73619249062986,1.42336732874239,-0.676899590973058));
#23886=CARTESIAN_POINT('Ctrl Pts',(-0.749495710301794,1.39534588636318,
-0.662390652284073));
#23887=CARTESIAN_POINT('Ctrl Pts',(-0.778498278845144,1.35110381617461,
-0.62804895077401));
#23888=CARTESIAN_POINT('Ctrl Pts',(-0.796153444118959,1.33188468517318,
-0.605884303066698));
#23889=CARTESIAN_POINT('Ctrl Pts',(-0.832065554235658,1.30632915724249,
-0.555538485325664));
#23890=CARTESIAN_POINT('Ctrl Pts',(-0.850258932191534,1.3,-0.527308329855003));
#23891=CARTESIAN_POINT('Ctrl Pts',(-0.881791875377343,1.3,-0.472691670144998));
#23892=CARTESIAN_POINT('Ctrl Pts',(-0.897143218189782,1.30632915724249,
-0.442820664919227));
#23893=CARTESIAN_POINT('Ctrl Pts',(-0.92278792026947,1.33188468517318,-0.386546956384144));
#23894=CARTESIAN_POINT('Ctrl Pts',(-0.933155485613026,1.35110381617461,
-0.360174810895352));
#23895=CARTESIAN_POINT('Ctrl Pts',(-0.948394987258249,1.39534588636318,
-0.31788699900678));
#23896=CARTESIAN_POINT('Ctrl Pts',(-0.954308486908894,1.42336732874239,
-0.299111603474268));
#23897=CARTESIAN_POINT('Ctrl Pts',(-0.961833761492986,1.48491957299737,
-0.273949373987484));
#23898=CARTESIAN_POINT('Ctrl Pts',(-0.963525491562421,1.5184626473304,-0.267616567329818));
#23899=CARTESIAN_POINT('Ctrl Pts',(-0.963525491562421,1.5815373526696,-0.267616567329818));
#23900=CARTESIAN_POINT('Ctrl Pts',(-0.961833761492986,1.61508042700263,
-0.273949373987484));
#23901=CARTESIAN_POINT('Ctrl Pts',(-0.954308486908894,1.67663267125761,
-0.299111603474268));
#23902=CARTESIAN_POINT('Ctrl Pts',(-0.948394987258249,1.70465411363682,
-0.31788699900678));
#23903=CARTESIAN_POINT('Ctrl Pts',(-0.933155485613026,1.74889618382539,
-0.360174810895352));
#23904=CARTESIAN_POINT('Ctrl Pts',(-0.92278792026947,1.76811531482682,-0.386546956384144));
#23905=CARTESIAN_POINT('Ctrl Pts',(-0.897143218189782,1.79367084275751,
-0.442820664919227));
#23906=CARTESIAN_POINT('Ctrl Pts',(-0.881791875377343,1.8,-0.472691670144998));
#23907=CARTESIAN_POINT('Ctrl Pts',(-0.850258932191534,1.8,-0.527308329855003));
#23908=CARTESIAN_POINT('Ctrl Pts',(-0.832065554235658,1.79367084275751,
-0.555538485325664));
#23909=CARTESIAN_POINT('Ctrl Pts',(-0.796153444118959,1.76811531482682,
-0.605884303066698));
#23910=CARTESIAN_POINT('Ctrl Pts',(-0.778498278845144,1.74889618382539,
-0.62804895077401));
#23911=CARTESIAN_POINT('Ctrl Pts',(-0.749495710301794,1.70465411363682,
-0.662390652284073));
#23912=CARTESIAN_POINT('Ctrl Pts',(-0.73619249062986,1.67663267125761,-0.676899590973058));
#23913=CARTESIAN_POINT('Ctrl Pts',(-0.718163997970498,1.61508042700263,
-0.695997784676728));
#23914=CARTESIAN_POINT('Ctrl Pts',(-0.713525491562421,1.5815373526696,-0.700629269222037));
#23915=CARTESIAN_POINT('Ctrl Pts',(-0.713525491562421,1.55,-0.700629269222037));
#23916=CARTESIAN_POINT('',(-1.28744468918255,1.55,-1.03198167246111));
#23917=CARTESIAN_POINT('',(0.125,1.55,-0.21650635094611));
#23918=CARTESIAN_POINT('',(-1.42894191624432,1.3,-0.825000000000001));
#23919=CARTESIAN_POINT('Ctrl Pts',(-1.42894191624432,1.3,-0.825000000000001));
#23920=CARTESIAN_POINT('Ctrl Pts',(-1.4132207435299,1.3,-0.852229869895949));
#23921=CARTESIAN_POINT('Ctrl Pts',(-1.39561049050871,1.30629366210296,-0.880751161609749));
#23922=CARTESIAN_POINT('Ctrl Pts',(-1.36172049302549,1.33182222741682,-0.932292094146256));
#23923=CARTESIAN_POINT('Ctrl Pts',(-1.34548213209931,1.35105447038507,-0.955340251466735));
#23924=CARTESIAN_POINT('Ctrl Pts',(-1.31917543061769,1.39539254159618,-0.991349264982991));
#23925=CARTESIAN_POINT('Ctrl Pts',(-1.30734972067592,1.42347183818157,-1.00672880483252));
#23926=CARTESIAN_POINT('Ctrl Pts',(-1.29146042158868,1.48505200040818,-1.02703269653942));
#23927=CARTESIAN_POINT('Ctrl Pts',(-1.28744468918255,1.51855708359447,-1.03198167246111));
#23928=CARTESIAN_POINT('Ctrl Pts',(-1.28744468918255,1.55,-1.03198167246111));
#23929=CARTESIAN_POINT('',(-1.42894191624432,1.8,-0.825000000000001));
#23930=CARTESIAN_POINT('Ctrl Pts',(-1.42894191624432,1.8,-0.825000000000001));
#23931=CARTESIAN_POINT('Ctrl Pts',(-1.44466308895875,1.8,-0.797770130104052));
#23932=CARTESIAN_POINT('Ctrl Pts',(-1.46055812562105,1.79370633789704,-0.768258557763732));
#23933=CARTESIAN_POINT('Ctrl Pts',(-1.48824888379079,1.76817777258318,-0.713138492740816));
#23934=CARTESIAN_POINT('Ctrl Pts',(-1.50008999307766,1.74894552961493,-0.687551581002689));
#23935=CARTESIAN_POINT('Ctrl Pts',(-1.51812136280714,1.70460745840382,-0.646764802471699));
#23936=CARTESIAN_POINT('Ctrl Pts',(-1.52552758004446,1.67652816181843,-0.628833667319578));
#23937=CARTESIAN_POINT('Ctrl Pts',(-1.53516661651472,1.61494799959182,-0.60492118480825));
#23938=CARTESIAN_POINT('Ctrl Pts',(-1.53744468918255,1.58144291640553,-0.598968970568896));
#23939=CARTESIAN_POINT('Ctrl Pts',(-1.53744468918255,1.51855708359447,-0.598968970568896));
#23940=CARTESIAN_POINT('Ctrl Pts',(-1.53516661651472,1.48505200040818,-0.60492118480825));
#23941=CARTESIAN_POINT('Ctrl Pts',(-1.52552758004446,1.42347183818157,-0.628833667319578));
#23942=CARTESIAN_POINT('Ctrl Pts',(-1.51812136280714,1.39539254159618,-0.646764802471699));
#23943=CARTESIAN_POINT('Ctrl Pts',(-1.50008999307766,1.35105447038507,-0.687551581002689));
#23944=CARTESIAN_POINT('Ctrl Pts',(-1.48824888379079,1.33182222741682,-0.713138492740816));
#23945=CARTESIAN_POINT('Ctrl Pts',(-1.46055812562105,1.30629366210296,-0.768258557763732));
#23946=CARTESIAN_POINT('Ctrl Pts',(-1.44466308895875,1.3,-0.797770130104052));
#23947=CARTESIAN_POINT('Ctrl Pts',(-1.42894191624432,1.3,-0.825000000000001));
#23948=CARTESIAN_POINT('Ctrl Pts',(-1.28744468918255,1.55,-1.03198167246111));
#23949=CARTESIAN_POINT('Ctrl Pts',(-1.28744468918255,1.58144291640553,-1.03198167246111));
#23950=CARTESIAN_POINT('Ctrl Pts',(-1.29146042158868,1.61494799959182,-1.02703269653942));
#23951=CARTESIAN_POINT('Ctrl Pts',(-1.30734972067592,1.67652816181843,-1.00672880483252));
#23952=CARTESIAN_POINT('Ctrl Pts',(-1.31917543061769,1.70460745840382,-0.991349264982991));
#23953=CARTESIAN_POINT('Ctrl Pts',(-1.34548213209931,1.74894552961493,-0.955340251466734));
#23954=CARTESIAN_POINT('Ctrl Pts',(-1.36172049302549,1.76817777258318,-0.932292094146256));
#23955=CARTESIAN_POINT('Ctrl Pts',(-1.39561049050871,1.79370633789704,-0.880751161609749));
#23956=CARTESIAN_POINT('Ctrl Pts',(-1.4132207435299,1.8,-0.852229869895949));
#23957=CARTESIAN_POINT('Ctrl Pts',(-1.42894191624432,1.8,-0.825000000000001));
#23958=CARTESIAN_POINT('Origin',(0.,1.55,0.));
#23959=CARTESIAN_POINT('',(-1.65,0.85,-2.02066721859313E-16));
#23960=CARTESIAN_POINT('Origin',(0.,0.85,0.));
#23961=CARTESIAN_POINT('',(-1.65,2.25,-2.02066721859313E-16));
#23962=CARTESIAN_POINT('',(-1.65,1.55,-2.02066721859313E-16));
#23963=CARTESIAN_POINT('Origin',(0.,2.25,0.));
#23964=CARTESIAN_POINT('',(-1.42894191624432,1.3,0.825));
#23965=CARTESIAN_POINT('',(-1.42894191624432,1.8,0.825));
#23966=CARTESIAN_POINT('Ctrl Pts',(-1.42894191624432,1.3,0.825));
#23967=CARTESIAN_POINT('Ctrl Pts',(-1.44466308895875,1.3,0.797770130104051));
#23968=CARTESIAN_POINT('Ctrl Pts',(-1.46055812562105,1.30629366210296,0.768258557763731));
#23969=CARTESIAN_POINT('Ctrl Pts',(-1.48824888379079,1.33182222741682,0.713138492740815));
#23970=CARTESIAN_POINT('Ctrl Pts',(-1.50008999307766,1.35105447038507,0.687551581002688));
#23971=CARTESIAN_POINT('Ctrl Pts',(-1.51812136280714,1.39539254159618,0.646764802471698));
#23972=CARTESIAN_POINT('Ctrl Pts',(-1.52552758004446,1.42347183818157,0.628833667319577));
#23973=CARTESIAN_POINT('Ctrl Pts',(-1.53516661651472,1.48505200040818,0.604921184808249));
#23974=CARTESIAN_POINT('Ctrl Pts',(-1.53744468918255,1.51855708359447,0.598968970568895));
#23975=CARTESIAN_POINT('Ctrl Pts',(-1.53744468918255,1.58144291640553,0.598968970568895));
#23976=CARTESIAN_POINT('Ctrl Pts',(-1.53516661651472,1.61494799959182,0.604921184808249));
#23977=CARTESIAN_POINT('Ctrl Pts',(-1.52552758004446,1.67652816181843,0.628833667319577));
#23978=CARTESIAN_POINT('Ctrl Pts',(-1.51812136280714,1.70460745840382,0.646764802471698));
#23979=CARTESIAN_POINT('Ctrl Pts',(-1.50008999307766,1.74894552961493,0.687551581002688));
#23980=CARTESIAN_POINT('Ctrl Pts',(-1.48824888379079,1.76817777258318,0.713138492740815));
#23981=CARTESIAN_POINT('Ctrl Pts',(-1.46055812562105,1.79370633789704,0.768258557763731));
#23982=CARTESIAN_POINT('Ctrl Pts',(-1.44466308895875,1.8,0.797770130104051));
#23983=CARTESIAN_POINT('Ctrl Pts',(-1.42894191624432,1.8,0.825));
#23984=CARTESIAN_POINT('',(-1.28744468918255,1.55,1.03198167246111));
#23985=CARTESIAN_POINT('Ctrl Pts',(-1.42894191624432,1.8,0.825));
#23986=CARTESIAN_POINT('Ctrl Pts',(-1.4132207435299,1.8,0.852229869895948));
#23987=CARTESIAN_POINT('Ctrl Pts',(-1.39561049050871,1.79370633789704,0.880751161609747));
#23988=CARTESIAN_POINT('Ctrl Pts',(-1.36172049302549,1.76817777258318,0.932292094146255));
#23989=CARTESIAN_POINT('Ctrl Pts',(-1.34548213209931,1.74894552961493,0.955340251466733));
#23990=CARTESIAN_POINT('Ctrl Pts',(-1.31917543061769,1.70460745840382,0.991349264982989));
#23991=CARTESIAN_POINT('Ctrl Pts',(-1.30734972067592,1.67652816181843,1.00672880483252));
#23992=CARTESIAN_POINT('Ctrl Pts',(-1.29146042158868,1.61494799959182,1.02703269653942));
#23993=CARTESIAN_POINT('Ctrl Pts',(-1.28744468918255,1.58144291640553,1.03198167246111));
#23994=CARTESIAN_POINT('Ctrl Pts',(-1.28744468918255,1.55,1.03198167246111));
#23995=CARTESIAN_POINT('Ctrl Pts',(-1.28744468918255,1.55,1.03198167246111));
#23996=CARTESIAN_POINT('Ctrl Pts',(-1.28744468918255,1.51855708359447,1.03198167246111));
#23997=CARTESIAN_POINT('Ctrl Pts',(-1.29146042158868,1.48505200040818,1.02703269653942));
#23998=CARTESIAN_POINT('Ctrl Pts',(-1.30734972067592,1.42347183818157,1.00672880483252));
#23999=CARTESIAN_POINT('Ctrl Pts',(-1.31917543061769,1.39539254159618,0.99134926498299));
#24000=CARTESIAN_POINT('Ctrl Pts',(-1.34548213209931,1.35105447038508,0.955340251466733));
#24001=CARTESIAN_POINT('Ctrl Pts',(-1.36172049302549,1.33182222741682,0.932292094146255));
#24002=CARTESIAN_POINT('Ctrl Pts',(-1.39561049050871,1.30629366210296,0.880751161609748));
#24003=CARTESIAN_POINT('Ctrl Pts',(-1.4132207435299,1.3,0.852229869895949));
#24004=CARTESIAN_POINT('Ctrl Pts',(-1.42894191624432,1.3,0.825));
#24005=CARTESIAN_POINT('',(1.42894191624432,1.8,-0.825));
#24006=CARTESIAN_POINT('',(1.42894191624432,1.3,-0.825));
#24007=CARTESIAN_POINT('Ctrl Pts',(1.42894191624432,1.8,-0.825));
#24008=CARTESIAN_POINT('Ctrl Pts',(1.4132207435299,1.8,-0.852229869895949));
#24009=CARTESIAN_POINT('Ctrl Pts',(1.39561049050871,1.79370633789704,-0.880751161609748));
#24010=CARTESIAN_POINT('Ctrl Pts',(1.36172049302549,1.76817777258318,-0.932292094146255));
#24011=CARTESIAN_POINT('Ctrl Pts',(1.34548213209931,1.74894552961493,-0.955340251466734));
#24012=CARTESIAN_POINT('Ctrl Pts',(1.31917543061769,1.70460745840382,-0.99134926498299));
#24013=CARTESIAN_POINT('Ctrl Pts',(1.30734972067592,1.67652816181843,-1.00672880483252));
#24014=CARTESIAN_POINT('Ctrl Pts',(1.29146042158868,1.61494799959182,-1.02703269653942));
#24015=CARTESIAN_POINT('Ctrl Pts',(1.28744468918255,1.58144291640553,-1.03198167246111));
#24016=CARTESIAN_POINT('Ctrl Pts',(1.28744468918255,1.51855708359447,-1.03198167246111));
#24017=CARTESIAN_POINT('Ctrl Pts',(1.29146042158868,1.48505200040818,-1.02703269653942));
#24018=CARTESIAN_POINT('Ctrl Pts',(1.30734972067592,1.42347183818157,-1.00672880483252));
#24019=CARTESIAN_POINT('Ctrl Pts',(1.31917543061769,1.39539254159618,-0.99134926498299));
#24020=CARTESIAN_POINT('Ctrl Pts',(1.34548213209931,1.35105447038507,-0.955340251466734));
#24021=CARTESIAN_POINT('Ctrl Pts',(1.36172049302549,1.33182222741682,-0.932292094146255));
#24022=CARTESIAN_POINT('Ctrl Pts',(1.39561049050871,1.30629366210296,-0.880751161609748));
#24023=CARTESIAN_POINT('Ctrl Pts',(1.4132207435299,1.3,-0.852229869895948));
#24024=CARTESIAN_POINT('Ctrl Pts',(1.42894191624432,1.3,-0.825));
#24025=CARTESIAN_POINT('',(1.53744468918255,1.55,-0.598968970568895));
#24026=CARTESIAN_POINT('Ctrl Pts',(1.42894191624432,1.3,-0.825));
#24027=CARTESIAN_POINT('Ctrl Pts',(1.44466308895875,1.3,-0.797770130104051));
#24028=CARTESIAN_POINT('Ctrl Pts',(1.46055812562105,1.30629366210296,-0.768258557763731));
#24029=CARTESIAN_POINT('Ctrl Pts',(1.48824888379079,1.33182222741682,-0.713138492740815));
#24030=CARTESIAN_POINT('Ctrl Pts',(1.50008999307766,1.35105447038507,-0.687551581002688));
#24031=CARTESIAN_POINT('Ctrl Pts',(1.51812136280714,1.39539254159618,-0.646764802471698));
#24032=CARTESIAN_POINT('Ctrl Pts',(1.52552758004446,1.42347183818157,-0.628833667319577));
#24033=CARTESIAN_POINT('Ctrl Pts',(1.53516661651472,1.48505200040818,-0.604921184808249));
#24034=CARTESIAN_POINT('Ctrl Pts',(1.53744468918255,1.51855708359447,-0.598968970568895));
#24035=CARTESIAN_POINT('Ctrl Pts',(1.53744468918255,1.55,-0.598968970568895));
#24036=CARTESIAN_POINT('Ctrl Pts',(1.53744468918255,1.55,-0.598968970568895));
#24037=CARTESIAN_POINT('Ctrl Pts',(1.53744468918255,1.58144291640553,-0.598968970568895));
#24038=CARTESIAN_POINT('Ctrl Pts',(1.53516661651472,1.61494799959182,-0.604921184808249));
#24039=CARTESIAN_POINT('Ctrl Pts',(1.52552758004446,1.67652816181843,-0.628833667319577));
#24040=CARTESIAN_POINT('Ctrl Pts',(1.51812136280714,1.70460745840382,-0.646764802471698));
#24041=CARTESIAN_POINT('Ctrl Pts',(1.50008999307766,1.74894552961493,-0.687551581002688));
#24042=CARTESIAN_POINT('Ctrl Pts',(1.48824888379079,1.76817777258318,-0.713138492740815));
#24043=CARTESIAN_POINT('Ctrl Pts',(1.46055812562105,1.79370633789704,-0.768258557763731));
#24044=CARTESIAN_POINT('Ctrl Pts',(1.44466308895875,1.8,-0.797770130104051));
#24045=CARTESIAN_POINT('Ctrl Pts',(1.42894191624432,1.8,-0.825));
#24046=CARTESIAN_POINT('',(0.,1.3,-1.65));
#24047=CARTESIAN_POINT('',(0.,1.8,-1.65));
#24048=CARTESIAN_POINT('Ctrl Pts',(1.38777878078145E-17,1.3,-1.65));
#24049=CARTESIAN_POINT('Ctrl Pts',(0.0314423454288489,1.3,-1.65));
#24050=CARTESIAN_POINT('Ctrl Pts',(0.0649476351123396,1.30629366210296,
-1.64900971937348));
#24051=CARTESIAN_POINT('Ctrl Pts',(0.126528390765307,1.33182222741682,-1.64543058688707));
#24052=CARTESIAN_POINT('Ctrl Pts',(0.154607860978348,1.35105447038507,-1.64289183246942));
#24053=CARTESIAN_POINT('Ctrl Pts',(0.198945932189457,1.39539254159618,-1.63811406745469));
#24054=CARTESIAN_POINT('Ctrl Pts',(0.218177859368546,1.42347183818157,-1.63556247215209));
#24055=CARTESIAN_POINT('Ctrl Pts',(0.243706194926033,1.48505200040818,-1.63195388134767));
#24056=CARTESIAN_POINT('Ctrl Pts',(0.25,1.51855708359447,-1.63095064303001));
#24057=CARTESIAN_POINT('Ctrl Pts',(0.25,1.58144291640553,-1.63095064303001));
#24058=CARTESIAN_POINT('Ctrl Pts',(0.243706194926033,1.61494799959182,-1.63195388134767));
#24059=CARTESIAN_POINT('Ctrl Pts',(0.218177859368546,1.67652816181843,-1.63556247215209));
#24060=CARTESIAN_POINT('Ctrl Pts',(0.198945932189457,1.70460745840382,-1.63811406745469));
#24061=CARTESIAN_POINT('Ctrl Pts',(0.154607860978349,1.74894552961493,-1.64289183246942));
#24062=CARTESIAN_POINT('Ctrl Pts',(0.126528390765307,1.76817777258318,-1.64543058688707));
#24063=CARTESIAN_POINT('Ctrl Pts',(0.0649476351123398,1.79370633789704,
-1.64900971937348));
#24064=CARTESIAN_POINT('Ctrl Pts',(0.031442345428849,1.8,-1.65));
#24065=CARTESIAN_POINT('Ctrl Pts',(7.63278329429795E-17,1.8,-1.65));
#24066=CARTESIAN_POINT('',(-0.25,1.55,-1.63095064303001));
#24067=CARTESIAN_POINT('Ctrl Pts',(9.0205620750794E-17,1.8,-1.65));
#24068=CARTESIAN_POINT('Ctrl Pts',(-0.0314423454288488,1.8,-1.65));
#24069=CARTESIAN_POINT('Ctrl Pts',(-0.0649476351123396,1.79370633789704,
-1.64900971937348));
#24070=CARTESIAN_POINT('Ctrl Pts',(-0.126528390765307,1.76817777258318,
-1.64543058688707));
#24071=CARTESIAN_POINT('Ctrl Pts',(-0.154607860978348,1.74894552961493,
-1.64289183246942));
#24072=CARTESIAN_POINT('Ctrl Pts',(-0.198945932189456,1.70460745840382,
-1.63811406745469));
#24073=CARTESIAN_POINT('Ctrl Pts',(-0.218177859368546,1.67652816181843,
-1.63556247215209));
#24074=CARTESIAN_POINT('Ctrl Pts',(-0.243706194926033,1.61494799959182,
-1.63195388134767));
#24075=CARTESIAN_POINT('Ctrl Pts',(-0.25,1.58144291640553,-1.63095064303001));
#24076=CARTESIAN_POINT('Ctrl Pts',(-0.25,1.55,-1.63095064303001));
#24077=CARTESIAN_POINT('Ctrl Pts',(-0.25,1.55,-1.63095064303001));
#24078=CARTESIAN_POINT('Ctrl Pts',(-0.25,1.51855708359447,-1.63095064303001));
#24079=CARTESIAN_POINT('Ctrl Pts',(-0.243706194926033,1.48505200040818,
-1.63195388134767));
#24080=CARTESIAN_POINT('Ctrl Pts',(-0.218177859368546,1.42347183818157,
-1.63556247215209));
#24081=CARTESIAN_POINT('Ctrl Pts',(-0.198945932189457,1.39539254159618,
-1.63811406745469));
#24082=CARTESIAN_POINT('Ctrl Pts',(-0.154607860978349,1.35105447038507,
-1.64289183246942));
#24083=CARTESIAN_POINT('Ctrl Pts',(-0.126528390765307,1.33182222741682,
-1.64543058688707));
#24084=CARTESIAN_POINT('Ctrl Pts',(-0.0649476351123398,1.30629366210296,
-1.64900971937348));
#24085=CARTESIAN_POINT('Ctrl Pts',(-0.031442345428849,1.3,-1.65));
#24086=CARTESIAN_POINT('Ctrl Pts',(-4.85722573273506E-17,1.3,-1.65));
#24087=CARTESIAN_POINT('',(0.,1.8,1.65));
#24088=CARTESIAN_POINT('',(0.,1.3,1.65));
#24089=CARTESIAN_POINT('Ctrl Pts',(8.32667268468867E-17,1.8,1.65));
#24090=CARTESIAN_POINT('Ctrl Pts',(0.031442345428849,1.8,1.65));
#24091=CARTESIAN_POINT('Ctrl Pts',(0.0649476351123398,1.79370633789704,
1.64900971937348));
#24092=CARTESIAN_POINT('Ctrl Pts',(0.126528390765307,1.76817777258318,1.64543058688707));
#24093=CARTESIAN_POINT('Ctrl Pts',(0.154607860978349,1.74894552961493,1.64289183246942));
#24094=CARTESIAN_POINT('Ctrl Pts',(0.198945932189457,1.70460745840382,1.63811406745469));
#24095=CARTESIAN_POINT('Ctrl Pts',(0.218177859368546,1.67652816181843,1.63556247215209));
#24096=CARTESIAN_POINT('Ctrl Pts',(0.243706194926033,1.61494799959182,1.63195388134767));
#24097=CARTESIAN_POINT('Ctrl Pts',(0.25,1.58144291640553,1.63095064303001));
#24098=CARTESIAN_POINT('Ctrl Pts',(0.25,1.51855708359447,1.63095064303001));
#24099=CARTESIAN_POINT('Ctrl Pts',(0.243706194926033,1.48505200040818,1.63195388134767));
#24100=CARTESIAN_POINT('Ctrl Pts',(0.218177859368546,1.42347183818157,1.63556247215209));
#24101=CARTESIAN_POINT('Ctrl Pts',(0.198945932189457,1.39539254159618,1.63811406745469));
#24102=CARTESIAN_POINT('Ctrl Pts',(0.154607860978348,1.35105447038507,1.64289183246942));
#24103=CARTESIAN_POINT('Ctrl Pts',(0.126528390765307,1.33182222741682,1.64543058688707));
#24104=CARTESIAN_POINT('Ctrl Pts',(0.0649476351123397,1.30629366210296,
1.64900971937348));
#24105=CARTESIAN_POINT('Ctrl Pts',(0.0314423454288488,1.3,1.65));
#24106=CARTESIAN_POINT('Ctrl Pts',(-1.38777878078145E-17,1.3,1.65));
#24107=CARTESIAN_POINT('',(-0.25,1.55,1.63095064303001));
#24108=CARTESIAN_POINT('Ctrl Pts',(-5.55111512312578E-17,1.3,1.65));
#24109=CARTESIAN_POINT('Ctrl Pts',(-0.031442345428849,1.3,1.65));
#24110=CARTESIAN_POINT('Ctrl Pts',(-0.0649476351123398,1.30629366210296,
1.64900971937348));
#24111=CARTESIAN_POINT('Ctrl Pts',(-0.126528390765307,1.33182222741682,
1.64543058688707));
#24112=CARTESIAN_POINT('Ctrl Pts',(-0.154607860978349,1.35105447038507,
1.64289183246942));
#24113=CARTESIAN_POINT('Ctrl Pts',(-0.198945932189457,1.39539254159618,
1.63811406745469));
#24114=CARTESIAN_POINT('Ctrl Pts',(-0.218177859368546,1.42347183818157,
1.63556247215209));
#24115=CARTESIAN_POINT('Ctrl Pts',(-0.243706194926033,1.48505200040818,
1.63195388134767));
#24116=CARTESIAN_POINT('Ctrl Pts',(-0.25,1.51855708359447,1.63095064303001));
#24117=CARTESIAN_POINT('Ctrl Pts',(-0.25,1.55,1.63095064303001));
#24118=CARTESIAN_POINT('Ctrl Pts',(-0.25,1.55,1.63095064303001));
#24119=CARTESIAN_POINT('Ctrl Pts',(-0.25,1.58144291640553,1.63095064303001));
#24120=CARTESIAN_POINT('Ctrl Pts',(-0.243706194926033,1.61494799959182,
1.63195388134767));
#24121=CARTESIAN_POINT('Ctrl Pts',(-0.218177859368546,1.67652816181843,
1.63556247215209));
#24122=CARTESIAN_POINT('Ctrl Pts',(-0.198945932189456,1.70460745840382,
1.63811406745469));
#24123=CARTESIAN_POINT('Ctrl Pts',(-0.154607860978348,1.74894552961493,
1.64289183246942));
#24124=CARTESIAN_POINT('Ctrl Pts',(-0.126528390765307,1.76817777258318,
1.64543058688707));
#24125=CARTESIAN_POINT('Ctrl Pts',(-0.0649476351123396,1.79370633789704,
1.64900971937348));
#24126=CARTESIAN_POINT('Ctrl Pts',(-0.0314423454288488,1.8,1.65));
#24127=CARTESIAN_POINT('Ctrl Pts',(7.63278329429795E-17,1.8,1.65));
#24128=CARTESIAN_POINT('Origin',(0.,1.55,0.));
#24129=CARTESIAN_POINT('',(-0.713525491562421,1.55,0.700629269222037));
#24130=CARTESIAN_POINT('',(0.125,1.55,0.21650635094611));
#24131=CARTESIAN_POINT('Ctrl Pts',(-0.713525491562421,1.55,0.700629269222037));
#24132=CARTESIAN_POINT('Ctrl Pts',(-0.713525491562421,1.5815373526696,0.700629269222037));
#24133=CARTESIAN_POINT('Ctrl Pts',(-0.718163997970498,1.61508042700263,
0.695997784676727));
#24134=CARTESIAN_POINT('Ctrl Pts',(-0.73619249062986,1.67663267125761,0.676899590973058));
#24135=CARTESIAN_POINT('Ctrl Pts',(-0.749495710301795,1.70465411363682,
0.662390652284073));
#24136=CARTESIAN_POINT('Ctrl Pts',(-0.778498278845144,1.74889618382539,
0.628048950774009));
#24137=CARTESIAN_POINT('Ctrl Pts',(-0.796153444118959,1.76811531482682,
0.605884303066698));
#24138=CARTESIAN_POINT('Ctrl Pts',(-0.832065554235658,1.79367084275751,
0.555538485325663));
#24139=CARTESIAN_POINT('Ctrl Pts',(-0.850258932191534,1.8,0.527308329855002));
#24140=CARTESIAN_POINT('Ctrl Pts',(-0.881791875377343,1.8,0.472691670144998));
#24141=CARTESIAN_POINT('Ctrl Pts',(-0.897143218189782,1.79367084275751,
0.442820664919227));
#24142=CARTESIAN_POINT('Ctrl Pts',(-0.92278792026947,1.76811531482682,0.386546956384144));
#24143=CARTESIAN_POINT('Ctrl Pts',(-0.933155485613026,1.74889618382539,
0.360174810895352));
#24144=CARTESIAN_POINT('Ctrl Pts',(-0.948394987258249,1.70465411363682,
0.31788699900678));
#24145=CARTESIAN_POINT('Ctrl Pts',(-0.954308486908894,1.67663267125761,
0.299111603474267));
#24146=CARTESIAN_POINT('Ctrl Pts',(-0.961833761492987,1.61508042700263,
0.273949373987484));
#24147=CARTESIAN_POINT('Ctrl Pts',(-0.963525491562421,1.5815373526696,0.267616567329817));
#24148=CARTESIAN_POINT('Ctrl Pts',(-0.963525491562421,1.5184626473304,0.267616567329817));
#24149=CARTESIAN_POINT('Ctrl Pts',(-0.961833761492987,1.48491957299737,
0.273949373987484));
#24150=CARTESIAN_POINT('Ctrl Pts',(-0.954308486908894,1.42336732874239,
0.299111603474267));
#24151=CARTESIAN_POINT('Ctrl Pts',(-0.948394987258249,1.39534588636318,
0.31788699900678));
#24152=CARTESIAN_POINT('Ctrl Pts',(-0.933155485613026,1.35110381617461,
0.360174810895352));
#24153=CARTESIAN_POINT('Ctrl Pts',(-0.92278792026947,1.33188468517318,0.386546956384144));
#24154=CARTESIAN_POINT('Ctrl Pts',(-0.897143218189782,1.30632915724249,
0.442820664919227));
#24155=CARTESIAN_POINT('Ctrl Pts',(-0.881791875377343,1.3,0.472691670144998));
#24156=CARTESIAN_POINT('Ctrl Pts',(-0.850258932191534,1.3,0.527308329855002));
#24157=CARTESIAN_POINT('Ctrl Pts',(-0.832065554235658,1.30632915724249,
0.555538485325663));
#24158=CARTESIAN_POINT('Ctrl Pts',(-0.796153444118959,1.33188468517318,
0.605884303066698));
#24159=CARTESIAN_POINT('Ctrl Pts',(-0.778498278845144,1.35110381617461,
0.628048950774009));
#24160=CARTESIAN_POINT('Ctrl Pts',(-0.749495710301795,1.39534588636318,
0.662390652284073));
#24161=CARTESIAN_POINT('Ctrl Pts',(-0.73619249062986,1.42336732874239,0.676899590973058));
#24162=CARTESIAN_POINT('Ctrl Pts',(-0.718163997970498,1.48491957299737,
0.695997784676727));
#24163=CARTESIAN_POINT('Ctrl Pts',(-0.713525491562421,1.5184626473304,0.700629269222037));
#24164=CARTESIAN_POINT('Ctrl Pts',(-0.713525491562421,1.55,0.700629269222037));
#24165=CARTESIAN_POINT('Origin',(0.,1.55,0.));
#24166=CARTESIAN_POINT('',(0.963525491562421,1.55,-0.267616567329817));
#24167=CARTESIAN_POINT('Ctrl Pts',(0.963525491562421,1.55,-0.267616567329817));
#24168=CARTESIAN_POINT('Ctrl Pts',(0.963525491562421,1.5184626473304,-0.267616567329817));
#24169=CARTESIAN_POINT('Ctrl Pts',(0.961833761492987,1.48491957299737,-0.273949373987484));
#24170=CARTESIAN_POINT('Ctrl Pts',(0.954308486908894,1.42336732874239,-0.299111603474267));
#24171=CARTESIAN_POINT('Ctrl Pts',(0.948394987258249,1.39534588636318,-0.31788699900678));
#24172=CARTESIAN_POINT('Ctrl Pts',(0.933155485613026,1.35110381617461,-0.360174810895352));
#24173=CARTESIAN_POINT('Ctrl Pts',(0.92278792026947,1.33188468517318,-0.386546956384144));
#24174=CARTESIAN_POINT('Ctrl Pts',(0.897143218189782,1.30632915724249,-0.442820664919227));
#24175=CARTESIAN_POINT('Ctrl Pts',(0.881791875377343,1.3,-0.472691670144998));
#24176=CARTESIAN_POINT('Ctrl Pts',(0.850258932191534,1.3,-0.527308329855002));
#24177=CARTESIAN_POINT('Ctrl Pts',(0.832065554235658,1.30632915724249,-0.555538485325663));
#24178=CARTESIAN_POINT('Ctrl Pts',(0.796153444118959,1.33188468517318,-0.605884303066698));
#24179=CARTESIAN_POINT('Ctrl Pts',(0.778498278845144,1.35110381617461,-0.628048950774009));
#24180=CARTESIAN_POINT('Ctrl Pts',(0.749495710301795,1.39534588636318,-0.662390652284073));
#24181=CARTESIAN_POINT('Ctrl Pts',(0.73619249062986,1.42336732874239,-0.676899590973058));
#24182=CARTESIAN_POINT('Ctrl Pts',(0.718163997970498,1.48491957299737,-0.695997784676727));
#24183=CARTESIAN_POINT('Ctrl Pts',(0.713525491562421,1.5184626473304,-0.700629269222037));
#24184=CARTESIAN_POINT('Ctrl Pts',(0.713525491562421,1.5815373526696,-0.700629269222037));
#24185=CARTESIAN_POINT('Ctrl Pts',(0.718163997970498,1.61508042700263,-0.695997784676727));
#24186=CARTESIAN_POINT('Ctrl Pts',(0.73619249062986,1.67663267125761,-0.676899590973058));
#24187=CARTESIAN_POINT('Ctrl Pts',(0.749495710301795,1.70465411363682,-0.662390652284073));
#24188=CARTESIAN_POINT('Ctrl Pts',(0.778498278845144,1.74889618382539,-0.628048950774009));
#24189=CARTESIAN_POINT('Ctrl Pts',(0.796153444118959,1.76811531482682,-0.605884303066698));
#24190=CARTESIAN_POINT('Ctrl Pts',(0.832065554235658,1.79367084275751,-0.555538485325663));
#24191=CARTESIAN_POINT('Ctrl Pts',(0.850258932191534,1.8,-0.527308329855002));
#24192=CARTESIAN_POINT('Ctrl Pts',(0.881791875377343,1.8,-0.472691670144998));
#24193=CARTESIAN_POINT('Ctrl Pts',(0.897143218189782,1.79367084275751,-0.442820664919227));
#24194=CARTESIAN_POINT('Ctrl Pts',(0.92278792026947,1.76811531482682,-0.386546956384144));
#24195=CARTESIAN_POINT('Ctrl Pts',(0.933155485613026,1.74889618382539,-0.360174810895352));
#24196=CARTESIAN_POINT('Ctrl Pts',(0.948394987258249,1.70465411363682,-0.31788699900678));
#24197=CARTESIAN_POINT('Ctrl Pts',(0.954308486908894,1.67663267125761,-0.299111603474267));
#24198=CARTESIAN_POINT('Ctrl Pts',(0.961833761492987,1.61508042700263,-0.273949373987484));
#24199=CARTESIAN_POINT('Ctrl Pts',(0.963525491562421,1.5815373526696,-0.267616567329817));
#24200=CARTESIAN_POINT('Ctrl Pts',(0.963525491562421,1.55,-0.267616567329817));
#24201=CARTESIAN_POINT('',(0.125,1.55,0.21650635094611));
#24202=CARTESIAN_POINT('Origin',(0.,1.55,0.));
#24203=CARTESIAN_POINT('',(-0.25,1.55,-0.968245836551854));
#24204=CARTESIAN_POINT('',(-0.25,1.55,0.));
#24205=CARTESIAN_POINT('Ctrl Pts',(-0.25,1.55,-0.968245836551854));
#24206=CARTESIAN_POINT('Ctrl Pts',(-0.25,1.5815373526696,-0.968245836551854));
#24207=CARTESIAN_POINT('Ctrl Pts',(-0.243669763522489,1.61508042700263,
-0.969947158664211));
#24208=CARTESIAN_POINT('Ctrl Pts',(-0.218115996279034,1.67663267125761,
-0.976011194447325));
#24209=CARTESIAN_POINT('Ctrl Pts',(-0.198899276956455,1.70465411363682,
-0.980277651290853));
#24210=CARTESIAN_POINT('Ctrl Pts',(-0.154657206767882,1.74889618382539,
-0.988223761669361));
#24211=CARTESIAN_POINT('Ctrl Pts',(-0.126634476150511,1.76811531482682,
-0.992431259450842));
#24212=CARTESIAN_POINT('Ctrl Pts',(-0.0650776639541238,1.79367084275751,
-0.99835915024489));
#24213=CARTESIAN_POINT('Ctrl Pts',(-0.0315329431858092,1.8,-1.));
#24214=CARTESIAN_POINT('Ctrl Pts',(0.0315329431858092,1.8,-1.));
#24215=CARTESIAN_POINT('Ctrl Pts',(0.0650776639541238,1.79367084275751,
-0.99835915024489));
#24216=CARTESIAN_POINT('Ctrl Pts',(0.126634476150511,1.76811531482682,-0.992431259450842));
#24217=CARTESIAN_POINT('Ctrl Pts',(0.154657206767882,1.74889618382539,-0.988223761669361));
#24218=CARTESIAN_POINT('Ctrl Pts',(0.198899276956455,1.70465411363682,-0.980277651290853));
#24219=CARTESIAN_POINT('Ctrl Pts',(0.218115996279034,1.67663267125761,-0.976011194447325));
#24220=CARTESIAN_POINT('Ctrl Pts',(0.243669763522488,1.61508042700263,-0.969947158664211));
#24221=CARTESIAN_POINT('Ctrl Pts',(0.25,1.5815373526696,-0.968245836551854));
#24222=CARTESIAN_POINT('Ctrl Pts',(0.25,1.5184626473304,-0.968245836551854));
#24223=CARTESIAN_POINT('Ctrl Pts',(0.243669763522488,1.48491957299737,-0.969947158664211));
#24224=CARTESIAN_POINT('Ctrl Pts',(0.218115996279034,1.42336732874239,-0.976011194447325));
#24225=CARTESIAN_POINT('Ctrl Pts',(0.198899276956455,1.39534588636318,-0.980277651290853));
#24226=CARTESIAN_POINT('Ctrl Pts',(0.154657206767882,1.35110381617461,-0.988223761669361));
#24227=CARTESIAN_POINT('Ctrl Pts',(0.126634476150511,1.33188468517318,-0.992431259450842));
#24228=CARTESIAN_POINT('Ctrl Pts',(0.0650776639541239,1.30632915724249,
-0.99835915024489));
#24229=CARTESIAN_POINT('Ctrl Pts',(0.0315329431858092,1.3,-1.));
#24230=CARTESIAN_POINT('Ctrl Pts',(-0.0315329431858092,1.3,-1.));
#24231=CARTESIAN_POINT('Ctrl Pts',(-0.0650776639541239,1.30632915724249,
-0.99835915024489));
#24232=CARTESIAN_POINT('Ctrl Pts',(-0.126634476150511,1.33188468517318,
-0.992431259450842));
#24233=CARTESIAN_POINT('Ctrl Pts',(-0.154657206767882,1.35110381617461,
-0.988223761669361));
#24234=CARTESIAN_POINT('Ctrl Pts',(-0.198899276956455,1.39534588636318,
-0.980277651290853));
#24235=CARTESIAN_POINT('Ctrl Pts',(-0.218115996279034,1.42336732874239,
-0.976011194447325));
#24236=CARTESIAN_POINT('Ctrl Pts',(-0.243669763522489,1.48491957299737,
-0.969947158664211));
#24237=CARTESIAN_POINT('Ctrl Pts',(-0.25,1.5184626473304,-0.968245836551854));
#24238=CARTESIAN_POINT('Ctrl Pts',(-0.25,1.55,-0.968245836551854));
#24239=CARTESIAN_POINT('Origin',(0.,1.55,0.));
#24240=CARTESIAN_POINT('',(-0.25,1.55,0.968245836551854));
#24241=CARTESIAN_POINT('Ctrl Pts',(-0.25,1.55,0.968245836551854));
#24242=CARTESIAN_POINT('Ctrl Pts',(-0.25,1.5184626473304,0.968245836551854));
#24243=CARTESIAN_POINT('Ctrl Pts',(-0.243669763522489,1.48491957299737,
0.969947158664211));
#24244=CARTESIAN_POINT('Ctrl Pts',(-0.218115996279034,1.42336732874239,
0.976011194447325));
#24245=CARTESIAN_POINT('Ctrl Pts',(-0.198899276956455,1.39534588636318,
0.980277651290853));
#24246=CARTESIAN_POINT('Ctrl Pts',(-0.154657206767882,1.35110381617461,
0.988223761669361));
#24247=CARTESIAN_POINT('Ctrl Pts',(-0.126634476150511,1.33188468517318,
0.992431259450842));
#24248=CARTESIAN_POINT('Ctrl Pts',(-0.065077663954124,1.30632915724249,
0.99835915024489));
#24249=CARTESIAN_POINT('Ctrl Pts',(-0.0315329431858092,1.3,1.));
#24250=CARTESIAN_POINT('Ctrl Pts',(0.0315329431858092,1.3,1.));
#24251=CARTESIAN_POINT('Ctrl Pts',(0.065077663954124,1.30632915724249,0.99835915024489));
#24252=CARTESIAN_POINT('Ctrl Pts',(0.126634476150511,1.33188468517318,0.992431259450842));
#24253=CARTESIAN_POINT('Ctrl Pts',(0.154657206767882,1.35110381617461,0.988223761669361));
#24254=CARTESIAN_POINT('Ctrl Pts',(0.198899276956455,1.39534588636318,0.980277651290853));
#24255=CARTESIAN_POINT('Ctrl Pts',(0.218115996279034,1.42336732874239,0.976011194447325));
#24256=CARTESIAN_POINT('Ctrl Pts',(0.243669763522488,1.48491957299737,0.969947158664211));
#24257=CARTESIAN_POINT('Ctrl Pts',(0.25,1.5184626473304,0.968245836551854));
#24258=CARTESIAN_POINT('Ctrl Pts',(0.25,1.5815373526696,0.968245836551854));
#24259=CARTESIAN_POINT('Ctrl Pts',(0.243669763522488,1.61508042700263,0.969947158664211));
#24260=CARTESIAN_POINT('Ctrl Pts',(0.218115996279034,1.67663267125761,0.976011194447325));
#24261=CARTESIAN_POINT('Ctrl Pts',(0.198899276956455,1.70465411363682,0.980277651290853));
#24262=CARTESIAN_POINT('Ctrl Pts',(0.154657206767882,1.74889618382539,0.988223761669361));
#24263=CARTESIAN_POINT('Ctrl Pts',(0.126634476150511,1.76811531482682,0.992431259450842));
#24264=CARTESIAN_POINT('Ctrl Pts',(0.0650776639541239,1.79367084275751,
0.99835915024489));
#24265=CARTESIAN_POINT('Ctrl Pts',(0.0315329431858092,1.8,1.));
#24266=CARTESIAN_POINT('Ctrl Pts',(-0.0315329431858092,1.8,1.));
#24267=CARTESIAN_POINT('Ctrl Pts',(-0.0650776639541239,1.79367084275751,
0.99835915024489));
#24268=CARTESIAN_POINT('Ctrl Pts',(-0.126634476150511,1.76811531482682,
0.992431259450842));
#24269=CARTESIAN_POINT('Ctrl Pts',(-0.154657206767882,1.74889618382539,
0.988223761669361));
#24270=CARTESIAN_POINT('Ctrl Pts',(-0.198899276956455,1.70465411363682,
0.980277651290853));
#24271=CARTESIAN_POINT('Ctrl Pts',(-0.218115996279034,1.67663267125761,
0.976011194447325));
#24272=CARTESIAN_POINT('Ctrl Pts',(-0.243669763522489,1.61508042700263,
0.969947158664211));
#24273=CARTESIAN_POINT('Ctrl Pts',(-0.25,1.5815373526696,0.968245836551854));
#24274=CARTESIAN_POINT('Ctrl Pts',(-0.25,1.55,0.968245836551854));
#24275=CARTESIAN_POINT('',(-0.25,1.55,0.));
#24276=CARTESIAN_POINT('Origin',(1.65,2.25,0.));
#24277=CARTESIAN_POINT('',(-1.,2.25,-1.22464679914735E-16));
#24278=CARTESIAN_POINT('Origin',(0.,2.25,0.));
#24279=CARTESIAN_POINT('Origin',(1.75,0.85,0.));
#24280=CARTESIAN_POINT('',(-1.75,0.85,-2.14313189850787E-16));
#24281=CARTESIAN_POINT('Origin',(0.,0.85,0.));
#24282=CARTESIAN_POINT('Origin',(0.,0.,0.));
#24283=CARTESIAN_POINT('',(-1.75,-0.85,-2.14313189850787E-16));
#24284=CARTESIAN_POINT('Origin',(0.,-0.85,0.));
#24285=CARTESIAN_POINT('',(-1.75,0.,-2.14313189850787E-16));
#24286=CARTESIAN_POINT('Origin',(1.,-0.85,0.));
#24287=CARTESIAN_POINT('',(-1.,-0.85,-1.22464679914735E-16));
#24288=CARTESIAN_POINT('Origin',(0.,-0.85,0.));
#24289=CARTESIAN_POINT('Origin',(0.,0.7,0.));
#24290=CARTESIAN_POINT('',(-1.,0.7,-1.22464679914735E-16));
#24291=CARTESIAN_POINT('',(0.,0.,0.));
#24292=CARTESIAN_POINT('',(0.,0.,0.));
#24293=CARTESIAN_POINT('',(0.,0.,0.));
#24294=CARTESIAN_POINT('Origin',(0.,0.,0.));
#24295=CARTESIAN_POINT('',(-0.42,0.16,5.14351655641888E-17));
#24296=CARTESIAN_POINT('Origin',(0.,0.16,0.));
#24297=CARTESIAN_POINT('',(-0.42,0.,5.14351655641888E-17));
#24298=CARTESIAN_POINT('',(-0.42,0.,5.14351655641888E-17));
#24299=CARTESIAN_POINT('Origin',(0.,0.,0.));
#24300=CARTESIAN_POINT('Origin',(0.,0.,0.));
#24301=CARTESIAN_POINT('',(-0.8,0.16,9.79717439317883E-17));
#24302=CARTESIAN_POINT('Origin',(0.,0.16,0.));
#24303=CARTESIAN_POINT('',(-0.8,0.,9.79717439317883E-17));
#24304=CARTESIAN_POINT('',(-0.8,0.,9.79717439317883E-17));
#24305=CARTESIAN_POINT('Origin',(0.,0.,0.));
#24306=CARTESIAN_POINT('Origin',(0.,0.16,0.));
#24307=CARTESIAN_POINT('Origin',(0.,0.,0.));
#24308=CARTESIAN_POINT('',(0.,0.,0.));
#24309=CARTESIAN_POINT('Origin',(0.173205080756888,-0.8,-0.3));
#24310=CARTESIAN_POINT('',(0.346410161513775,-0.8,0.));
#24311=CARTESIAN_POINT('',(0.173205080756888,-0.8,-0.3));
#24312=CARTESIAN_POINT('',(0.346410161513775,-0.8,0.));
#24313=CARTESIAN_POINT('',(0.173205080756888,-1.28,-0.3));
#24314=CARTESIAN_POINT('',(0.173205080756888,-0.8,-0.3));
#24315=CARTESIAN_POINT('',(0.346410161513775,-1.28,0.));
#24316=CARTESIAN_POINT('',(0.346410161513775,-1.28,0.));
#24317=CARTESIAN_POINT('',(0.346410161513775,-0.8,0.));
#24318=CARTESIAN_POINT('Origin',(-0.173205080756888,-0.8,-0.3));
#24319=CARTESIAN_POINT('',(-0.173205080756888,-0.8,-0.3));
#24320=CARTESIAN_POINT('',(0.173205080756888,-0.8,-0.3));
#24321=CARTESIAN_POINT('',(-0.173205080756888,-1.28,-0.3));
#24322=CARTESIAN_POINT('',(-0.173205080756888,-0.8,-0.3));
#24323=CARTESIAN_POINT('',(0.173205080756888,-1.28,-0.3));
#24324=CARTESIAN_POINT('Origin',(-0.346410161513775,-0.8,-5.55111512312578E-17));
#24325=CARTESIAN_POINT('',(-0.346410161513775,-0.8,-4.24230095489963E-17));
#24326=CARTESIAN_POINT('',(-0.173205080756888,-0.8,-0.3));
#24327=CARTESIAN_POINT('',(-0.346410161513775,-1.28,-5.55111512312578E-17));
#24328=CARTESIAN_POINT('',(-0.346410161513775,-0.8,-4.24230095489963E-17));
#24329=CARTESIAN_POINT('',(-0.173205080756888,-1.28,-0.3));
#24330=CARTESIAN_POINT('Origin',(-0.173205080756888,-0.8,0.3));
#24331=CARTESIAN_POINT('',(-0.173205080756888,-0.8,0.3));
#24332=CARTESIAN_POINT('',(-0.346410161513775,-0.8,-4.24230095489963E-17));
#24333=CARTESIAN_POINT('',(-0.173205080756888,-1.28,0.3));
#24334=CARTESIAN_POINT('',(-0.173205080756888,-0.8,0.3));
#24335=CARTESIAN_POINT('',(-0.346410161513775,-1.28,-4.24230095489963E-17));
#24336=CARTESIAN_POINT('Origin',(0.173205080756888,-0.8,0.3));
#24337=CARTESIAN_POINT('',(0.173205080756888,-0.8,0.3));
#24338=CARTESIAN_POINT('',(-0.173205080756888,-0.8,0.3));
#24339=CARTESIAN_POINT('',(0.173205080756888,-1.28,0.3));
#24340=CARTESIAN_POINT('',(0.173205080756888,-0.8,0.3));
#24341=CARTESIAN_POINT('',(-0.173205080756888,-1.28,0.3));
#24342=CARTESIAN_POINT('Origin',(0.346410161513775,-0.8,0.));
#24343=CARTESIAN_POINT('',(0.173205080756888,-0.8,0.3));
#24344=CARTESIAN_POINT('',(0.173205080756888,-1.28,0.3));
#24345=CARTESIAN_POINT('Origin',(0.,-0.8,-5.55111512312578E-17));
#24346=CARTESIAN_POINT('Origin',(0.,-1.28,-5.55111512312578E-17));
#24347=CARTESIAN_POINT('Origin',(0.,-2.5,0.));
#24348=CARTESIAN_POINT('',(-0.3933,-2.5,4.81653586104654E-17));
#24349=CARTESIAN_POINT('Origin',(0.,-2.5,0.));
#24350=CARTESIAN_POINT('Origin',(0.6,0.8,0.));
#24351=CARTESIAN_POINT('',(-0.6,0.8,-7.34788079488412E-17));
#24352=CARTESIAN_POINT('Origin',(0.,0.8,0.));
#24353=CARTESIAN_POINT('Origin',(0.,0.775,0.));
#24354=CARTESIAN_POINT('',(-0.65,0.75,-7.9602041944578E-17));
#24355=CARTESIAN_POINT('Origin',(0.,0.75,0.));
#24356=CARTESIAN_POINT('',(-0.625,0.775,-7.65404249467096E-17));
#24357=CARTESIAN_POINT('Origin',(0.,0.39,0.));
#24358=CARTESIAN_POINT('',(-0.65,0.0299999999999998,-7.9602041944578E-17));
#24359=CARTESIAN_POINT('Origin',(0.,0.0299999999999998,0.));
#24360=CARTESIAN_POINT('',(-0.65,0.39,-7.9602041944578E-17));
#24361=CARTESIAN_POINT('Origin',(0.,0.0150000000000001,0.));
#24362=CARTESIAN_POINT('',(-0.62,5.89805981832114E-17,-7.59281015471359E-17));
#24363=CARTESIAN_POINT('Origin',(0.,0.,0.));
#24364=CARTESIAN_POINT('',(-0.635,0.0150000000000001,-7.77650717458569E-17));
#24365=CARTESIAN_POINT('Origin',(0.42,0.,0.));
#24366=CARTESIAN_POINT('',(-0.42,-3.46944695195361E-18,-5.14351655641888E-17));
#24367=CARTESIAN_POINT('Origin',(0.,0.,0.));
#24368=CARTESIAN_POINT('Origin',(0.,-0.02,0.));
#24369=CARTESIAN_POINT('',(-0.3933,-0.0534000000000001,4.81653586104654E-17));
#24370=CARTESIAN_POINT('Origin',(0.,-0.0534000000000001,0.));
#24371=CARTESIAN_POINT('',(-0.41,-0.02,-5.02105187650415E-17));
#24372=CARTESIAN_POINT('Origin',(0.,-1.48,0.));
#24373=CARTESIAN_POINT('',(-0.3933,-1.48,-4.81653586104654E-17));
#24374=CARTESIAN_POINT('',(0.,0.,0.));
#24375=CARTESIAN_POINT('Origin',(0.0866025403784439,-0.4,-0.15));
#24376=CARTESIAN_POINT('',(0.173205080756888,-0.4,0.));
#24377=CARTESIAN_POINT('',(0.0866025403784439,-0.4,-0.15));
#24378=CARTESIAN_POINT('',(0.173205080756888,-0.4,0.));
#24379=CARTESIAN_POINT('',(0.0866025403784439,-0.64,-0.15));
#24380=CARTESIAN_POINT('',(0.0866025403784439,-0.4,-0.15));
#24381=CARTESIAN_POINT('',(0.173205080756888,-0.64,0.));
#24382=CARTESIAN_POINT('',(0.173205080756888,-0.64,0.));
#24383=CARTESIAN_POINT('',(0.173205080756888,-0.4,0.));
#24384=CARTESIAN_POINT('Origin',(-0.0866025403784438,-0.4,-0.15));
#24385=CARTESIAN_POINT('',(-0.0866025403784438,-0.4,-0.15));
#24386=CARTESIAN_POINT('',(0.0866025403784439,-0.4,-0.15));
#24387=CARTESIAN_POINT('',(-0.0866025403784438,-0.64,-0.15));
#24388=CARTESIAN_POINT('',(-0.0866025403784438,-0.4,-0.15));
#24389=CARTESIAN_POINT('',(0.0866025403784439,-0.64,-0.15));
#24390=CARTESIAN_POINT('Origin',(-0.173205080756888,-0.4,-2.77555756156289E-17));
#24391=CARTESIAN_POINT('',(-0.173205080756888,-0.4,-2.12115047744981E-17));
#24392=CARTESIAN_POINT('',(-0.0866025403784438,-0.4,-0.15));
#24393=CARTESIAN_POINT('',(-0.173205080756888,-0.64,-2.77555756156289E-17));
#24394=CARTESIAN_POINT('',(-0.173205080756888,-0.4,-2.12115047744981E-17));
#24395=CARTESIAN_POINT('',(-0.0866025403784438,-0.64,-0.15));
#24396=CARTESIAN_POINT('Origin',(-0.0866025403784439,-0.4,0.15));
#24397=CARTESIAN_POINT('',(-0.0866025403784439,-0.4,0.15));
#24398=CARTESIAN_POINT('',(-0.173205080756888,-0.4,-2.12115047744981E-17));
#24399=CARTESIAN_POINT('',(-0.0866025403784439,-0.64,0.15));
#24400=CARTESIAN_POINT('',(-0.0866025403784439,-0.4,0.15));
#24401=CARTESIAN_POINT('',(-0.173205080756888,-0.64,-2.12115047744981E-17));
#24402=CARTESIAN_POINT('Origin',(0.0866025403784439,-0.4,0.15));
#24403=CARTESIAN_POINT('',(0.0866025403784439,-0.4,0.15));
#24404=CARTESIAN_POINT('',(-0.0866025403784439,-0.4,0.15));
#24405=CARTESIAN_POINT('',(0.0866025403784439,-0.64,0.15));
#24406=CARTESIAN_POINT('',(0.0866025403784439,-0.4,0.15));
#24407=CARTESIAN_POINT('',(-0.0866025403784439,-0.64,0.15));
#24408=CARTESIAN_POINT('Origin',(0.173205080756888,-0.4,0.));
#24409=CARTESIAN_POINT('',(0.0866025403784439,-0.4,0.15));
#24410=CARTESIAN_POINT('',(0.0866025403784439,-0.64,0.15));
#24411=CARTESIAN_POINT('Origin',(0.,-0.4,-2.77555756156289E-17));
#24412=CARTESIAN_POINT('Origin',(0.,-0.64,-2.77555756156289E-17));
#24413=CARTESIAN_POINT('Origin',(0.,-1.,0.));
#24414=CARTESIAN_POINT('',(-0.1954,-1.,2.39295984553393E-17));
#24415=CARTESIAN_POINT('Origin',(0.,-1.,0.));
#24416=CARTESIAN_POINT('Origin',(0.3,0.4,0.));
#24417=CARTESIAN_POINT('',(-0.3,0.4,-3.67394039744206E-17));
#24418=CARTESIAN_POINT('Origin',(0.,0.4,0.));
#24419=CARTESIAN_POINT('Origin',(0.,0.375,0.));
#24420=CARTESIAN_POINT('',(-0.35,0.35,-4.28626379701573E-17));
#24421=CARTESIAN_POINT('Origin',(0.,0.35,0.));
#24422=CARTESIAN_POINT('',(-0.325,0.375,-3.9801020972289E-17));
#24423=CARTESIAN_POINT('Origin',(0.,0.19,0.));
#24424=CARTESIAN_POINT('',(-0.35,0.03,-4.28626379701574E-17));
#24425=CARTESIAN_POINT('Origin',(0.,0.03,0.));
#24426=CARTESIAN_POINT('',(-0.35,0.19,-4.28626379701574E-17));
#24427=CARTESIAN_POINT('Origin',(0.,0.0149999999999999,0.));
#24428=CARTESIAN_POINT('',(-0.32,-3.29597460435593E-17,-3.91886975727153E-17));
#24429=CARTESIAN_POINT('Origin',(0.,0.,0.));
#24430=CARTESIAN_POINT('',(-0.335,0.0149999999999999,-4.10256677714363E-17));
#24431=CARTESIAN_POINT('Origin',(0.22,0.,0.));
#24432=CARTESIAN_POINT('',(-0.22,-6.93889390390723E-18,-2.69422295812418E-17));
#24433=CARTESIAN_POINT('Origin',(0.,0.,0.));
#24434=CARTESIAN_POINT('Origin',(0.,-0.02,0.));
#24435=CARTESIAN_POINT('',(-0.1954,-0.0492,2.39295984553393E-17));
#24436=CARTESIAN_POINT('Origin',(0.,-0.0492,0.));
#24437=CARTESIAN_POINT('',(-0.21,-0.02,-2.57175827820944E-17));
#24438=CARTESIAN_POINT('Origin',(0.,-0.8,0.));
#24439=CARTESIAN_POINT('',(-0.1954,-0.8,-2.39295984553393E-17));
#24440=CARTESIAN_POINT('',(0.,0.,0.));
#24441=CARTESIAN_POINT('',(0.,0.,0.));
#24442=CARTESIAN_POINT('Origin',(0.,-5.1,7.));
#24443=CARTESIAN_POINT('',(-0.165,-5.,7.));
#24444=CARTESIAN_POINT('Origin',(0.,-5.,7.));
#24445=CARTESIAN_POINT('',(-0.165,-3.4,7.));
#24446=CARTESIAN_POINT('',(-0.165,-5.1,7.));
#24447=CARTESIAN_POINT('Origin',(0.,-3.4,7.));
#24448=CARTESIAN_POINT('Origin',(0.,-3.4,7.));
#24449=CARTESIAN_POINT('Origin',(0.,2.05,7.));
#24450=CARTESIAN_POINT('',(-0.7,2.05,7.));
#24451=CARTESIAN_POINT('Origin',(0.,2.05,7.));
#24452=CARTESIAN_POINT('',(-0.5,2.05,7.));
#24453=CARTESIAN_POINT('Origin',(0.,2.05,7.));
#24454=CARTESIAN_POINT('Origin',(0.,1.35,7.));
#24455=CARTESIAN_POINT('',(-0.7,1.35,7.));
#24456=CARTESIAN_POINT('Origin',(0.,1.35,7.));
#24457=CARTESIAN_POINT('',(-0.5,1.35,7.));
#24458=CARTESIAN_POINT('Origin',(0.,1.35,7.));
#24459=CARTESIAN_POINT('Origin',(0.,1.35,7.));
#24460=CARTESIAN_POINT('',(-0.7,1.35,7.));
#24461=CARTESIAN_POINT('Origin',(0.,-1.8,7.));
#24462=CARTESIAN_POINT('',(-0.5,-1.8,7.));
#24463=CARTESIAN_POINT('',(-0.5,-1.8,7.));
#24464=CARTESIAN_POINT('Origin',(0.,-1.8,7.));
#24465=CARTESIAN_POINT('Origin',(0.,-5.,7.));
#24466=CARTESIAN_POINT('',(-0.4,-1.8,7.));
#24467=CARTESIAN_POINT('Origin',(0.,-1.8,7.));
#24468=CARTESIAN_POINT('',(-0.4,-5.,7.));
#24469=CARTESIAN_POINT('',(-0.4,-5.,7.));
#24470=CARTESIAN_POINT('Origin',(0.,-5.,7.));
#24471=CARTESIAN_POINT('Origin',(0.,-5.,7.));
#24472=CARTESIAN_POINT('Origin',(0.,-1.8,7.));
#24473=CARTESIAN_POINT('',(-0.5,3.,7.));
#24474=CARTESIAN_POINT('Origin',(0.,3.,7.));
#24475=CARTESIAN_POINT('',(-0.5,-1.8,7.));
#24476=CARTESIAN_POINT('Origin',(0.,3.,7.));
#24477=CARTESIAN_POINT('Origin',(0.,-1.8,7.));
#24478=CARTESIAN_POINT('',(0.,0.,0.));
#24479=CARTESIAN_POINT('Origin',(0.,-1.8,7.));
#24480=CARTESIAN_POINT('',(-0.505,-1.8,7.));
#24481=CARTESIAN_POINT('Origin',(0.,-1.8,7.));
#24482=CARTESIAN_POINT('',(-0.505,-1.35,7.));
#24483=CARTESIAN_POINT('',(-0.505,-1.8,7.));
#24484=CARTESIAN_POINT('Origin',(0.,-1.35,7.));
#24485=CARTESIAN_POINT('Origin',(0.,-1.8,7.));
#24486=CARTESIAN_POINT('',(-0.405,-1.8,7.));
#24487=CARTESIAN_POINT('Origin',(0.,-1.8,7.));
#24488=CARTESIAN_POINT('Origin',(0.,-2.65,7.));
#24489=CARTESIAN_POINT('',(-0.405,-2.65,7.));
#24490=CARTESIAN_POINT('',(-0.405,-2.65,7.));
#24491=CARTESIAN_POINT('Origin',(0.,-2.65,7.));
#24492=CARTESIAN_POINT('Origin',(0.,-2.65,7.));
#24493=CARTESIAN_POINT('',(-0.7,-1.35,7.));
#24494=CARTESIAN_POINT('Origin',(0.,-1.35,7.));
#24495=CARTESIAN_POINT('',(-0.7,-2.65,7.));
#24496=CARTESIAN_POINT('',(-0.7,-2.65,7.));
#24497=CARTESIAN_POINT('Origin',(0.,-2.65,7.));
#24498=CARTESIAN_POINT('Origin',(0.,-1.35,7.));
#24499=CARTESIAN_POINT('Origin',(0.,-2.65,7.));
#24500=CARTESIAN_POINT('',(0.,0.,0.));
#24501=CARTESIAN_POINT('Origin',(0.,-0.45,7.));
#24502=CARTESIAN_POINT('',(-0.505,0.45,7.));
#24503=CARTESIAN_POINT('Origin',(0.,0.45,7.));
#24504=CARTESIAN_POINT('',(-0.505,-0.45,7.));
#24505=CARTESIAN_POINT('',(-0.505,-0.45,7.));
#24506=CARTESIAN_POINT('Origin',(0.,-0.45,7.));
#24507=CARTESIAN_POINT('Origin',(0.,-0.45,7.));
#24508=CARTESIAN_POINT('',(-0.7,0.45,7.));
#24509=CARTESIAN_POINT('Origin',(0.,0.45,7.));
#24510=CARTESIAN_POINT('',(-0.7,-0.45,7.));
#24511=CARTESIAN_POINT('',(-0.7,-0.45,7.));
#24512=CARTESIAN_POINT('Origin',(0.,-0.45,7.));
#24513=CARTESIAN_POINT('Origin',(0.,0.45,7.));
#24514=CARTESIAN_POINT('Origin',(0.,-0.45,7.));
#24515=CARTESIAN_POINT('',(0.,0.,0.));
#24516=CARTESIAN_POINT('Origin',(0.,-3.95,6.35));
#24517=CARTESIAN_POINT('',(-0.15,-3.95,6.6));
#24518=CARTESIAN_POINT('Origin',(0.,-3.95,6.6));
#24519=CARTESIAN_POINT('',(-0.15,-3.95,6.35));
#24520=CARTESIAN_POINT('',(-0.15,-3.95,6.35));
#24521=CARTESIAN_POINT('Origin',(0.,-3.95,6.35));
#24522=CARTESIAN_POINT('Origin',(0.,-3.95,6.6));
#24523=CARTESIAN_POINT('Origin',(0.,-3.95,6.35));
#24524=CARTESIAN_POINT('',(0.,0.,0.));
#24525=CARTESIAN_POINT('Origin',(0.,-3.95,7.4));
#24526=CARTESIAN_POINT('',(-0.15,-3.95,7.65));
#24527=CARTESIAN_POINT('Origin',(0.,-3.95,7.65));
#24528=CARTESIAN_POINT('',(-0.15,-3.95,7.4));
#24529=CARTESIAN_POINT('',(-0.15,-3.95,7.4));
#24530=CARTESIAN_POINT('Origin',(0.,-3.95,7.4));
#24531=CARTESIAN_POINT('Origin',(0.,-3.95,7.65));
#24532=CARTESIAN_POINT('Origin',(0.,-3.95,7.4));
#24533=CARTESIAN_POINT('',(0.,0.,0.));
#24534=CARTESIAN_POINT('Origin',(0.,-5.2,7.));
#24535=CARTESIAN_POINT('',(-0.225,-5.,7.));
#24536=CARTESIAN_POINT('Origin',(0.,-5.,7.));
#24537=CARTESIAN_POINT('',(-0.225,-5.2,7.));
#24538=CARTESIAN_POINT('',(-0.225,-5.2,7.));
#24539=CARTESIAN_POINT('Origin',(0.,-5.2,7.));
#24540=CARTESIAN_POINT('Origin',(0.,-5.2,7.));
#24541=CARTESIAN_POINT('',(-0.6,-5.,7.));
#24542=CARTESIAN_POINT('Origin',(0.,-5.,7.));
#24543=CARTESIAN_POINT('',(-0.6,-5.2,7.));
#24544=CARTESIAN_POINT('',(-0.6,-5.2,7.));
#24545=CARTESIAN_POINT('Origin',(0.,-5.2,7.));
#24546=CARTESIAN_POINT('Origin',(0.,-5.,7.));
#24547=CARTESIAN_POINT('Origin',(0.,-5.2,7.));
#24548=CARTESIAN_POINT('',(0.,0.,0.));
#24549=CARTESIAN_POINT('Origin',(0.,3.,7.));
#24550=CARTESIAN_POINT('',(-0.5,5.,7.));
#24551=CARTESIAN_POINT('Origin',(0.,5.,7.));
#24552=CARTESIAN_POINT('',(-0.5,3.,7.));
#24553=CARTESIAN_POINT('',(-0.5,3.,7.));
#24554=CARTESIAN_POINT('Origin',(0.,3.,7.));
#24555=CARTESIAN_POINT('Origin',(0.,5.,7.));
#24556=CARTESIAN_POINT('Origin',(0.,3.,7.));
#24557=CARTESIAN_POINT('',(0.,0.,0.));
#24558=CARTESIAN_POINT('Origin',(0.,3.5,7.49));
#24559=CARTESIAN_POINT('',(0.122167917228702,3.32919309147461,7.49));
#24560=CARTESIAN_POINT('',(0.122167917228702,3.67080690852539,7.49));
#24561=CARTESIAN_POINT('',(0.122167917228702,2.1,7.49));
#24562=CARTESIAN_POINT('Origin',(0.,3.5,7.49));
#24563=CARTESIAN_POINT('Origin',(0.,3.5,7.49));
#24564=CARTESIAN_POINT('',(-0.122167917228702,3.32919309147461,7.49));
#24565=CARTESIAN_POINT('Ctrl Pts',(-0.122167917228702,3.32919309147461,
7.49));
#24566=CARTESIAN_POINT('Ctrl Pts',(-0.109498349122107,3.3201313107707,7.49315880560769));
#24567=CARTESIAN_POINT('Ctrl Pts',(-0.0955290239036627,3.31230742432584,
7.49610638003428));
#24568=CARTESIAN_POINT('Ctrl Pts',(-0.0549836006623198,3.29540341787373,
7.50267917175998));
#24569=CARTESIAN_POINT('Ctrl Pts',(-0.0267085342178658,3.29,7.505));
#24570=CARTESIAN_POINT('Ctrl Pts',(0.0267085342178659,3.29,7.505));
#24571=CARTESIAN_POINT('Ctrl Pts',(0.0549836006623198,3.29540341787373,
7.50267917175998));
#24572=CARTESIAN_POINT('Ctrl Pts',(0.0955290239036627,3.31230742432584,
7.49610638003428));
#24573=CARTESIAN_POINT('Ctrl Pts',(0.109498349122108,3.3201313107707,7.49315880560769));
#24574=CARTESIAN_POINT('Ctrl Pts',(0.122167917228702,3.32919309147461,7.49));
#24575=CARTESIAN_POINT('',(-0.21,3.5,7.49));
#24576=CARTESIAN_POINT('Origin',(0.,3.5,7.49));
#24577=CARTESIAN_POINT('',(-0.21,3.5,7.97770138590472));
#24578=CARTESIAN_POINT('',(-0.21,3.5,7.49));
#24579=CARTESIAN_POINT('',(0.21,3.5,7.97770138590472));
#24580=CARTESIAN_POINT('Ctrl Pts',(0.21,3.5,7.97770138590472));
#24581=CARTESIAN_POINT('Ctrl Pts',(0.21,3.47354611741017,7.97770138590472));
#24582=CARTESIAN_POINT('Ctrl Pts',(0.204697017125528,3.44538474169131,7.97888646613217));
#24583=CARTESIAN_POINT('Ctrl Pts',(0.183241751515529,3.39366957869826,7.98312869991148));
#24584=CARTESIAN_POINT('Ctrl Pts',(0.167093586802906,3.37010873870456,7.98612044796649));
#24585=CARTESIAN_POINT('Ctrl Pts',(0.129892533236543,3.33290768513819,7.99170645156379));
#24586=CARTESIAN_POINT('Ctrl Pts',(0.106331154992714,3.31675852489431,7.99466914446598));
#24587=CARTESIAN_POINT('Ctrl Pts',(0.0546141143983531,3.29530253627557,
7.99884449237241));
#24588=CARTESIAN_POINT('Ctrl Pts',(0.0264520736824499,3.29,8.));
#24589=CARTESIAN_POINT('Ctrl Pts',(-0.0264520736824498,3.29,8.));
#24590=CARTESIAN_POINT('Ctrl Pts',(-0.054614114398353,3.29530253627557,
7.99884449237241));
#24591=CARTESIAN_POINT('Ctrl Pts',(-0.106331154992714,3.31675852489431,
7.99466914446598));
#24592=CARTESIAN_POINT('Ctrl Pts',(-0.129892533236543,3.33290768513819,
7.99170645156379));
#24593=CARTESIAN_POINT('Ctrl Pts',(-0.167093586802906,3.37010873870456,
7.98612044796649));
#24594=CARTESIAN_POINT('Ctrl Pts',(-0.183241751515529,3.39366957869826,
7.98312869991148));
#24595=CARTESIAN_POINT('Ctrl Pts',(-0.204697017125528,3.44538474169131,
7.97888646613217));
#24596=CARTESIAN_POINT('Ctrl Pts',(-0.21,3.47354611741017,7.97770138590472));
#24597=CARTESIAN_POINT('Ctrl Pts',(-0.21,3.5,7.97770138590472));
#24598=CARTESIAN_POINT('Ctrl Pts',(-0.21,3.5,7.97770138590472));
#24599=CARTESIAN_POINT('Ctrl Pts',(-0.21,3.52645388258983,7.97770138590472));
#24600=CARTESIAN_POINT('Ctrl Pts',(-0.204697017125528,3.55461525830869,
7.97888646613217));
#24601=CARTESIAN_POINT('Ctrl Pts',(-0.183241751515529,3.60633042130174,
7.98312869991148));
#24602=CARTESIAN_POINT('Ctrl Pts',(-0.167093586802906,3.62989126129544,
7.98612044796649));
#24603=CARTESIAN_POINT('Ctrl Pts',(-0.129892533236543,3.66709231486181,
7.99170645156379));
#24604=CARTESIAN_POINT('Ctrl Pts',(-0.106331154992714,3.68324147510569,
7.99466914446598));
#24605=CARTESIAN_POINT('Ctrl Pts',(-0.0546141143983532,3.70469746372443,
7.99884449237241));
#24606=CARTESIAN_POINT('Ctrl Pts',(-0.0264520736824499,3.71,8.));
#24607=CARTESIAN_POINT('Ctrl Pts',(0.0264520736824498,3.71,8.));
#24608=CARTESIAN_POINT('Ctrl Pts',(0.0546141143983531,3.70469746372443,
7.99884449237241));
#24609=CARTESIAN_POINT('Ctrl Pts',(0.106331154992714,3.68324147510569,7.99466914446598));
#24610=CARTESIAN_POINT('Ctrl Pts',(0.129892533236543,3.66709231486181,7.99170645156379));
#24611=CARTESIAN_POINT('Ctrl Pts',(0.167093586802906,3.62989126129544,7.98612044796649));
#24612=CARTESIAN_POINT('Ctrl Pts',(0.183241751515529,3.60633042130174,7.98312869991148));
#24613=CARTESIAN_POINT('Ctrl Pts',(0.204697017125528,3.55461525830869,7.97888646613217));
#24614=CARTESIAN_POINT('Ctrl Pts',(0.21,3.52645388258983,7.97770138590472));
#24615=CARTESIAN_POINT('Ctrl Pts',(0.21,3.5,7.97770138590472));
#24616=CARTESIAN_POINT('',(-0.122167917228702,3.67080690852539,7.49));
#24617=CARTESIAN_POINT('Origin',(0.,3.5,7.49));
#24618=CARTESIAN_POINT('Ctrl Pts',(0.122167917228702,3.67080690852539,7.49));
#24619=CARTESIAN_POINT('Ctrl Pts',(0.109498349122108,3.6798686892293,7.49315880560769));
#24620=CARTESIAN_POINT('Ctrl Pts',(0.0955290239036627,3.68769257567416,
7.49610638003428));
#24621=CARTESIAN_POINT('Ctrl Pts',(0.0549836006623198,3.70459658212627,
7.50267917175998));
#24622=CARTESIAN_POINT('Ctrl Pts',(0.0267085342178658,3.71,7.505));
#24623=CARTESIAN_POINT('Ctrl Pts',(-0.0267085342178659,3.71,7.505));
#24624=CARTESIAN_POINT('Ctrl Pts',(-0.0549836006623198,3.70459658212627,
7.50267917175998));
#24625=CARTESIAN_POINT('Ctrl Pts',(-0.0955290239036627,3.68769257567416,
7.49610638003428));
#24626=CARTESIAN_POINT('Ctrl Pts',(-0.109498349122107,3.6798686892293,7.49315880560769));
#24627=CARTESIAN_POINT('Ctrl Pts',(-0.122167917228702,3.67080690852539,
7.49));
#24628=CARTESIAN_POINT('Origin',(0.,3.5,7.49));
#24629=CARTESIAN_POINT('',(-0.122167917228702,2.1,7.49));
#24630=CARTESIAN_POINT('Origin',(0.,2.5,7.49));
#24631=CARTESIAN_POINT('',(0.122167917228702,2.32919309147461,7.49));
#24632=CARTESIAN_POINT('',(0.122167917228702,2.67080690852539,7.49));
#24633=CARTESIAN_POINT('',(0.122167917228702,2.1,7.49));
#24634=CARTESIAN_POINT('Origin',(0.,2.5,7.49));
#24635=CARTESIAN_POINT('Origin',(0.,2.5,7.49));
#24636=CARTESIAN_POINT('',(-0.122167917228702,2.32919309147461,7.49));
#24637=CARTESIAN_POINT('Ctrl Pts',(-0.122167917228702,2.32919309147461,
7.49));
#24638=CARTESIAN_POINT('Ctrl Pts',(-0.109498349122107,2.3201313107707,7.49315880560769));
#24639=CARTESIAN_POINT('Ctrl Pts',(-0.0955290239036627,2.31230742432584,
7.49610638003428));
#24640=CARTESIAN_POINT('Ctrl Pts',(-0.0549836006623198,2.29540341787373,
7.50267917175998));
#24641=CARTESIAN_POINT('Ctrl Pts',(-0.0267085342178658,2.29,7.505));
#24642=CARTESIAN_POINT('Ctrl Pts',(0.0267085342178659,2.29,7.505));
#24643=CARTESIAN_POINT('Ctrl Pts',(0.0549836006623198,2.29540341787373,
7.50267917175998));
#24644=CARTESIAN_POINT('Ctrl Pts',(0.0955290239036627,2.31230742432584,
7.49610638003428));
#24645=CARTESIAN_POINT('Ctrl Pts',(0.109498349122107,2.3201313107707,7.49315880560769));
#24646=CARTESIAN_POINT('Ctrl Pts',(0.122167917228702,2.32919309147461,7.49));
#24647=CARTESIAN_POINT('',(-0.21,2.5,7.49));
#24648=CARTESIAN_POINT('Origin',(0.,2.5,7.49));
#24649=CARTESIAN_POINT('',(-0.21,2.5,7.97770138590472));
#24650=CARTESIAN_POINT('',(-0.21,2.5,7.49));
#24651=CARTESIAN_POINT('',(0.21,2.5,7.97770138590472));
#24652=CARTESIAN_POINT('Ctrl Pts',(0.21,2.5,7.97770138590472));
#24653=CARTESIAN_POINT('Ctrl Pts',(0.21,2.47354611741017,7.97770138590472));
#24654=CARTESIAN_POINT('Ctrl Pts',(0.204697017125528,2.44538474169131,7.97888646613217));
#24655=CARTESIAN_POINT('Ctrl Pts',(0.183241751515529,2.39366957869826,7.98312869991148));
#24656=CARTESIAN_POINT('Ctrl Pts',(0.167093586802906,2.37010873870456,7.98612044796649));
#24657=CARTESIAN_POINT('Ctrl Pts',(0.129892533236543,2.33290768513819,7.99170645156379));
#24658=CARTESIAN_POINT('Ctrl Pts',(0.106331154992714,2.31675852489431,7.99466914446598));
#24659=CARTESIAN_POINT('Ctrl Pts',(0.0546141143983531,2.29530253627557,
7.99884449237241));
#24660=CARTESIAN_POINT('Ctrl Pts',(0.0264520736824499,2.29,8.));
#24661=CARTESIAN_POINT('Ctrl Pts',(-0.0264520736824498,2.29,8.));
#24662=CARTESIAN_POINT('Ctrl Pts',(-0.0546141143983532,2.29530253627557,
7.99884449237241));
#24663=CARTESIAN_POINT('Ctrl Pts',(-0.106331154992714,2.31675852489431,
7.99466914446598));
#24664=CARTESIAN_POINT('Ctrl Pts',(-0.129892533236543,2.33290768513819,
7.99170645156379));
#24665=CARTESIAN_POINT('Ctrl Pts',(-0.167093586802906,2.37010873870456,
7.98612044796649));
#24666=CARTESIAN_POINT('Ctrl Pts',(-0.183241751515529,2.39366957869826,
7.98312869991148));
#24667=CARTESIAN_POINT('Ctrl Pts',(-0.204697017125528,2.44538474169131,
7.97888646613217));
#24668=CARTESIAN_POINT('Ctrl Pts',(-0.21,2.47354611741017,7.97770138590472));
#24669=CARTESIAN_POINT('Ctrl Pts',(-0.21,2.5,7.97770138590472));
#24670=CARTESIAN_POINT('Ctrl Pts',(-0.21,2.5,7.97770138590472));
#24671=CARTESIAN_POINT('Ctrl Pts',(-0.21,2.52645388258983,7.97770138590472));
#24672=CARTESIAN_POINT('Ctrl Pts',(-0.204697017125528,2.55461525830869,
7.97888646613217));
#24673=CARTESIAN_POINT('Ctrl Pts',(-0.183241751515529,2.60633042130174,
7.98312869991148));
#24674=CARTESIAN_POINT('Ctrl Pts',(-0.167093586802906,2.62989126129544,
7.98612044796649));
#24675=CARTESIAN_POINT('Ctrl Pts',(-0.129892533236543,2.66709231486181,
7.99170645156379));
#24676=CARTESIAN_POINT('Ctrl Pts',(-0.106331154992714,2.68324147510569,
7.99466914446598));
#24677=CARTESIAN_POINT('Ctrl Pts',(-0.0546141143983532,2.70469746372443,
7.99884449237241));
#24678=CARTESIAN_POINT('Ctrl Pts',(-0.0264520736824499,2.71,8.));
#24679=CARTESIAN_POINT('Ctrl Pts',(0.0264520736824498,2.71,8.));
#24680=CARTESIAN_POINT('Ctrl Pts',(0.0546141143983531,2.70469746372443,
7.99884449237241));
#24681=CARTESIAN_POINT('Ctrl Pts',(0.106331154992714,2.68324147510569,7.99466914446598));
#24682=CARTESIAN_POINT('Ctrl Pts',(0.129892533236543,2.66709231486181,7.99170645156379));
#24683=CARTESIAN_POINT('Ctrl Pts',(0.167093586802906,2.62989126129544,7.98612044796649));
#24684=CARTESIAN_POINT('Ctrl Pts',(0.183241751515529,2.60633042130174,7.98312869991148));
#24685=CARTESIAN_POINT('Ctrl Pts',(0.204697017125528,2.55461525830869,7.97888646613217));
#24686=CARTESIAN_POINT('Ctrl Pts',(0.21,2.52645388258983,7.97770138590472));
#24687=CARTESIAN_POINT('Ctrl Pts',(0.21,2.5,7.97770138590472));
#24688=CARTESIAN_POINT('',(-0.122167917228702,2.67080690852539,7.49));
#24689=CARTESIAN_POINT('Origin',(0.,2.5,7.49));
#24690=CARTESIAN_POINT('Ctrl Pts',(0.122167917228702,2.67080690852539,7.49));
#24691=CARTESIAN_POINT('Ctrl Pts',(0.109498349122107,2.6798686892293,7.49315880560769));
#24692=CARTESIAN_POINT('Ctrl Pts',(0.0955290239036627,2.68769257567416,
7.49610638003428));
#24693=CARTESIAN_POINT('Ctrl Pts',(0.0549836006623198,2.70459658212627,
7.50267917175998));
#24694=CARTESIAN_POINT('Ctrl Pts',(0.0267085342178658,2.71,7.505));
#24695=CARTESIAN_POINT('Ctrl Pts',(-0.0267085342178659,2.71,7.505));
#24696=CARTESIAN_POINT('Ctrl Pts',(-0.0549836006623198,2.70459658212627,
7.50267917175998));
#24697=CARTESIAN_POINT('Ctrl Pts',(-0.0955290239036626,2.68769257567416,
7.49610638003428));
#24698=CARTESIAN_POINT('Ctrl Pts',(-0.109498349122107,2.6798686892293,7.49315880560769));
#24699=CARTESIAN_POINT('Ctrl Pts',(-0.122167917228702,2.67080690852539,
7.49));
#24700=CARTESIAN_POINT('Origin',(0.,2.5,7.49));
#24701=CARTESIAN_POINT('',(-0.122167917228702,2.1,7.49));
#24702=CARTESIAN_POINT('Origin',(0.,2.1,7.));
#24703=CARTESIAN_POINT('',(-0.505,4.,7.));
#24704=CARTESIAN_POINT('Origin',(0.,4.,7.));
#24705=CARTESIAN_POINT('',(-0.505,2.1,7.));
#24706=CARTESIAN_POINT('',(-0.505,2.1,7.));
#24707=CARTESIAN_POINT('Origin',(0.,2.1,7.));
#24708=CARTESIAN_POINT('Origin',(0.,2.1,7.));
#24709=CARTESIAN_POINT('',(-1.,4.,7.));
#24710=CARTESIAN_POINT('Origin',(0.,4.,7.));
#24711=CARTESIAN_POINT('',(-1.,2.1,7.));
#24712=CARTESIAN_POINT('',(-1.,2.1,7.));
#24713=CARTESIAN_POINT('Origin',(0.,2.1,7.));
#24714=CARTESIAN_POINT('Origin',(0.,4.,7.));
#24715=CARTESIAN_POINT('Origin',(0.,2.1,7.));
#24716=CARTESIAN_POINT('',(0.,0.,0.));
#24717=CARTESIAN_POINT('Origin',(0.,-0.45,0.));
#24718=CARTESIAN_POINT('',(-0.65,-0.325,-3.9801020972289E-17));
#24719=CARTESIAN_POINT('',(-0.637867541108654,-0.45,0.125));
#24720=CARTESIAN_POINT('Ctrl Pts',(-0.65,-0.325,-6.93889390390723E-17));
#24721=CARTESIAN_POINT('Ctrl Pts',(-0.65,-0.325,0.0157371373481997));
#24722=CARTESIAN_POINT('Ctrl Pts',(-0.649370620646074,-0.328153081062251,
0.0324967135411163));
#24723=CARTESIAN_POINT('Ctrl Pts',(-0.647096224417991,-0.340922081922822,
0.0632828231545122));
#24724=CARTESIAN_POINT('Ctrl Pts',(-0.645482573914132,-0.350535859112198,
0.0773125544088347));
#24725=CARTESIAN_POINT('Ctrl Pts',(-0.642442040715078,-0.372687974598127,
0.0994646698947638));
#24726=CARTESIAN_POINT('Ctrl Pts',(-0.640815160902589,-0.386717480603274,
0.109078032552995));
#24727=CARTESIAN_POINT('Ctrl Pts',(-0.63851034608138,-0.417502809542363,
0.121846732641678));
#24728=CARTESIAN_POINT('Ctrl Pts',(-0.637867541108654,-0.434262111007648,
0.125));
#24729=CARTESIAN_POINT('Ctrl Pts',(-0.637867541108654,-0.45,0.125));
#24730=CARTESIAN_POINT('',(-0.65,-0.575,-3.9801020972289E-17));
#24731=CARTESIAN_POINT('Ctrl Pts',(-0.65,-0.575,-3.46944695195361E-18));
#24732=CARTESIAN_POINT('Ctrl Pts',(-0.65,-0.575,-0.0157371373481998));
#24733=CARTESIAN_POINT('Ctrl Pts',(-0.649370620646074,-0.571846918937749,
-0.0324967135411164));
#24734=CARTESIAN_POINT('Ctrl Pts',(-0.647096224417991,-0.559077918077178,
-0.0632828231545123));
#24735=CARTESIAN_POINT('Ctrl Pts',(-0.645482573914132,-0.549464140887802,
-0.0773125544088349));
#24736=CARTESIAN_POINT('Ctrl Pts',(-0.642442040715078,-0.527312025401873,
-0.099464669894764));
#24737=CARTESIAN_POINT('Ctrl Pts',(-0.640815160902589,-0.513282519396725,
-0.109078032552995));
#24738=CARTESIAN_POINT('Ctrl Pts',(-0.63851034608138,-0.482497190457637,
-0.121846732641678));
#24739=CARTESIAN_POINT('Ctrl Pts',(-0.637867541108654,-0.465737888992352,
-0.125));
#24740=CARTESIAN_POINT('Ctrl Pts',(-0.637867541108654,-0.434262111007648,
-0.125));
#24741=CARTESIAN_POINT('Ctrl Pts',(-0.63851034608138,-0.417502809542363,
-0.121846732641678));
#24742=CARTESIAN_POINT('Ctrl Pts',(-0.640815160902589,-0.386717480603275,
-0.109078032552995));
#24743=CARTESIAN_POINT('Ctrl Pts',(-0.642442040715078,-0.372687974598127,
-0.099464669894764));
#24744=CARTESIAN_POINT('Ctrl Pts',(-0.645482573914132,-0.350535859112198,
-0.077312554408835));
#24745=CARTESIAN_POINT('Ctrl Pts',(-0.647096224417991,-0.340922081922822,
-0.0632828231545124));
#24746=CARTESIAN_POINT('Ctrl Pts',(-0.649370620646074,-0.328153081062251,
-0.0324967135411165));
#24747=CARTESIAN_POINT('Ctrl Pts',(-0.65,-0.325,-0.0157371373481999));
#24748=CARTESIAN_POINT('Ctrl Pts',(-0.65,-0.325,-8.32667268468867E-17));
#24749=CARTESIAN_POINT('Ctrl Pts',(-0.637867541108654,-0.45,0.125));
#24750=CARTESIAN_POINT('Ctrl Pts',(-0.637867541108654,-0.465737888992352,
0.125));
#24751=CARTESIAN_POINT('Ctrl Pts',(-0.63851034608138,-0.482497190457637,
0.121846732641678));
#24752=CARTESIAN_POINT('Ctrl Pts',(-0.640815160902589,-0.513282519396725,
0.109078032552995));
#24753=CARTESIAN_POINT('Ctrl Pts',(-0.642442040715078,-0.527312025401873,
0.0994646698947639));
#24754=CARTESIAN_POINT('Ctrl Pts',(-0.645482573914132,-0.549464140887802,
0.0773125544088349));
#24755=CARTESIAN_POINT('Ctrl Pts',(-0.647096224417991,-0.559077918077178,
0.0632828231545123));
#24756=CARTESIAN_POINT('Ctrl Pts',(-0.649370620646074,-0.571846918937749,
0.0324967135411164));
#24757=CARTESIAN_POINT('Ctrl Pts',(-0.65,-0.575,0.0157371373481998));
#24758=CARTESIAN_POINT('Ctrl Pts',(-0.65,-0.575,-2.08166817117217E-17));
#24759=CARTESIAN_POINT('',(-0.379967103839267,-0.45,0.125));
#24760=CARTESIAN_POINT('',(-7.65404249467096E-18,-0.45,0.125));
#24761=CARTESIAN_POINT('',(-0.4,-0.575,5.41097774720219E-18));
#24762=CARTESIAN_POINT('Ctrl Pts',(-0.4,-0.575,-3.81639164714898E-17));
#24763=CARTESIAN_POINT('Ctrl Pts',(-0.4,-0.575,0.0158075115832675));
#24764=CARTESIAN_POINT('Ctrl Pts',(-0.398970551469948,-0.571819306519379,
0.0325978607437828));
#24765=CARTESIAN_POINT('Ctrl Pts',(-0.395252954914593,-0.559029081159106,
0.0633657881355917));
#24766=CARTESIAN_POINT('Ctrl Pts',(-0.392612801026882,-0.549425200318011,
0.0773514949786256));
#24767=CARTESIAN_POINT('Ctrl Pts',(-0.38761064154154,-0.527347592689753,
0.0994291026068839));
#24768=CARTESIAN_POINT('Ctrl Pts',(-0.384911758361269,-0.51336346023721,
0.109029967924066));
#24769=CARTESIAN_POINT('Ctrl Pts',(-0.381057715344782,-0.48260129709332,
0.121817958968287));
#24770=CARTESIAN_POINT('Ctrl Pts',(-0.379967103839267,-0.465813100629203,
0.125));
#24771=CARTESIAN_POINT('Ctrl Pts',(-0.379967103839267,-0.45,0.125));
#24772=CARTESIAN_POINT('',(-0.379967103839267,-0.45,-0.125));
#24773=CARTESIAN_POINT('Ctrl Pts',(-0.379967103839267,-0.45,-0.125));
#24774=CARTESIAN_POINT('Ctrl Pts',(-0.379967103839267,-0.465813100629203,
-0.125));
#24775=CARTESIAN_POINT('Ctrl Pts',(-0.381057715344782,-0.48260129709332,
-0.121817958968287));
#24776=CARTESIAN_POINT('Ctrl Pts',(-0.384911758361269,-0.51336346023721,
-0.109029967924066));
#24777=CARTESIAN_POINT('Ctrl Pts',(-0.38761064154154,-0.527347592689753,
-0.099429102606884));
#24778=CARTESIAN_POINT('Ctrl Pts',(-0.392612801026882,-0.549425200318011,
-0.0773514949786257));
#24779=CARTESIAN_POINT('Ctrl Pts',(-0.395252954914593,-0.559029081159106,
-0.0633657881355918));
#24780=CARTESIAN_POINT('Ctrl Pts',(-0.398970551469948,-0.571819306519379,
-0.0325978607437828));
#24781=CARTESIAN_POINT('Ctrl Pts',(-0.4,-0.575,-0.0158075115832676));
#24782=CARTESIAN_POINT('Ctrl Pts',(-0.4,-0.575,-4.16333634234434E-17));
#24783=CARTESIAN_POINT('',(-0.4,-0.325,2.96971064108775E-17));
#24784=CARTESIAN_POINT('Ctrl Pts',(-0.4,-0.325,1.04083408558608E-17));
#24785=CARTESIAN_POINT('Ctrl Pts',(-0.4,-0.325,-0.0158075115832676));
#24786=CARTESIAN_POINT('Ctrl Pts',(-0.398970551469948,-0.328180693480621,
-0.0325978607437828));
#24787=CARTESIAN_POINT('Ctrl Pts',(-0.395252954914593,-0.340970918840894,
-0.0633657881355918));
#24788=CARTESIAN_POINT('Ctrl Pts',(-0.392612801026882,-0.350574799681989,
-0.0773514949786256));
#24789=CARTESIAN_POINT('Ctrl Pts',(-0.38761064154154,-0.372652407310247,
-0.0994291026068839));
#24790=CARTESIAN_POINT('Ctrl Pts',(-0.384911758361269,-0.38663653976279,
-0.109029967924066));
#24791=CARTESIAN_POINT('Ctrl Pts',(-0.381057715344782,-0.41739870290668,
-0.121817958968287));
#24792=CARTESIAN_POINT('Ctrl Pts',(-0.379967103839267,-0.434186899370797,
-0.125));
#24793=CARTESIAN_POINT('Ctrl Pts',(-0.379967103839267,-0.45,-0.125));
#24794=CARTESIAN_POINT('Ctrl Pts',(-0.379967103839267,-0.45,0.125));
#24795=CARTESIAN_POINT('Ctrl Pts',(-0.379967103839267,-0.434186899370797,
0.125));
#24796=CARTESIAN_POINT('Ctrl Pts',(-0.381057715344782,-0.41739870290668,
0.121817958968287));
#24797=CARTESIAN_POINT('Ctrl Pts',(-0.384911758361269,-0.38663653976279,
0.109029967924066));
#24798=CARTESIAN_POINT('Ctrl Pts',(-0.38761064154154,-0.372652407310247,
0.0994291026068839));
#24799=CARTESIAN_POINT('Ctrl Pts',(-0.392612801026882,-0.350574799681989,
0.0773514949786257));
#24800=CARTESIAN_POINT('Ctrl Pts',(-0.395252954914593,-0.340970918840894,
0.0633657881355918));
#24801=CARTESIAN_POINT('Ctrl Pts',(-0.398970551469948,-0.328180693480621,
0.0325978607437829));
#24802=CARTESIAN_POINT('Ctrl Pts',(-0.4,-0.325,0.0158075115832676));
#24803=CARTESIAN_POINT('Ctrl Pts',(-0.4,-0.325,1.38777878078145E-17));
#24804=CARTESIAN_POINT('Origin',(0.,-0.45,0.));
#24805=CARTESIAN_POINT('',(0.379967103839267,-0.45,-0.125));
#24806=CARTESIAN_POINT('',(0.379967103839267,-0.45,0.125));
#24807=CARTESIAN_POINT('Ctrl Pts',(0.379967103839267,-0.45,-0.125));
#24808=CARTESIAN_POINT('Ctrl Pts',(0.379967103839267,-0.434186899370797,
-0.125));
#24809=CARTESIAN_POINT('Ctrl Pts',(0.381057715344782,-0.41739870290668,
-0.121817958968287));
#24810=CARTESIAN_POINT('Ctrl Pts',(0.384911758361269,-0.38663653976279,
-0.109029967924066));
#24811=CARTESIAN_POINT('Ctrl Pts',(0.38761064154154,-0.372652407310247,
-0.0994291026068839));
#24812=CARTESIAN_POINT('Ctrl Pts',(0.392612801026882,-0.350574799681989,
-0.0773514949786256));
#24813=CARTESIAN_POINT('Ctrl Pts',(0.395252954914593,-0.340970918840894,
-0.0633657881355917));
#24814=CARTESIAN_POINT('Ctrl Pts',(0.398970551469948,-0.328180693480621,
-0.0325978607437828));
#24815=CARTESIAN_POINT('Ctrl Pts',(0.4,-0.325,-0.0158075115832675));
#24816=CARTESIAN_POINT('Ctrl Pts',(0.4,-0.325,0.0158075115832676));
#24817=CARTESIAN_POINT('Ctrl Pts',(0.398970551469948,-0.328180693480621,
0.0325978607437829));
#24818=CARTESIAN_POINT('Ctrl Pts',(0.395252954914593,-0.340970918840894,
0.0633657881355918));
#24819=CARTESIAN_POINT('Ctrl Pts',(0.392612801026882,-0.350574799681989,
0.0773514949786257));
#24820=CARTESIAN_POINT('Ctrl Pts',(0.38761064154154,-0.372652407310247,
0.099429102606884));
#24821=CARTESIAN_POINT('Ctrl Pts',(0.384911758361269,-0.38663653976279,
0.109029967924066));
#24822=CARTESIAN_POINT('Ctrl Pts',(0.381057715344782,-0.41739870290668,
0.121817958968287));
#24823=CARTESIAN_POINT('Ctrl Pts',(0.379967103839267,-0.434186899370797,
0.125));
#24824=CARTESIAN_POINT('Ctrl Pts',(0.379967103839267,-0.45,0.125));
#24825=CARTESIAN_POINT('Ctrl Pts',(0.379967103839267,-0.45,0.125));
#24826=CARTESIAN_POINT('Ctrl Pts',(0.379967103839267,-0.465813100629203,
0.125));
#24827=CARTESIAN_POINT('Ctrl Pts',(0.381057715344782,-0.48260129709332,
0.121817958968287));
#24828=CARTESIAN_POINT('Ctrl Pts',(0.384911758361269,-0.51336346023721,
0.109029967924066));
#24829=CARTESIAN_POINT('Ctrl Pts',(0.38761064154154,-0.527347592689753,
0.0994291026068839));
#24830=CARTESIAN_POINT('Ctrl Pts',(0.392612801026882,-0.549425200318011,
0.0773514949786257));
#24831=CARTESIAN_POINT('Ctrl Pts',(0.395252954914593,-0.559029081159106,
0.0633657881355918));
#24832=CARTESIAN_POINT('Ctrl Pts',(0.398970551469948,-0.571819306519379,
0.0325978607437829));
#24833=CARTESIAN_POINT('Ctrl Pts',(0.4,-0.575,0.0158075115832676));
#24834=CARTESIAN_POINT('Ctrl Pts',(0.4,-0.575,-0.0158075115832676));
#24835=CARTESIAN_POINT('Ctrl Pts',(0.398970551469948,-0.57181930651938,
-0.0325978607437828));
#24836=CARTESIAN_POINT('Ctrl Pts',(0.395252954914593,-0.559029081159106,
-0.0633657881355918));
#24837=CARTESIAN_POINT('Ctrl Pts',(0.392612801026882,-0.549425200318011,
-0.0773514949786257));
#24838=CARTESIAN_POINT('Ctrl Pts',(0.38761064154154,-0.527347592689753,
-0.0994291026068839));
#24839=CARTESIAN_POINT('Ctrl Pts',(0.384911758361269,-0.51336346023721,
-0.109029967924066));
#24840=CARTESIAN_POINT('Ctrl Pts',(0.381057715344782,-0.48260129709332,
-0.121817958968287));
#24841=CARTESIAN_POINT('Ctrl Pts',(0.379967103839267,-0.465813100629203,
-0.125));
#24842=CARTESIAN_POINT('Ctrl Pts',(0.379967103839267,-0.45,-0.125));
#24843=CARTESIAN_POINT('',(0.637867541108654,-0.45,0.125));
#24844=CARTESIAN_POINT('',(-7.65404249467096E-18,-0.45,0.125));
#24845=CARTESIAN_POINT('',(0.65,-0.575,3.9801020972289E-17));
#24846=CARTESIAN_POINT('Ctrl Pts',(0.65,-0.575,5.55111512312578E-17));
#24847=CARTESIAN_POINT('Ctrl Pts',(0.65,-0.575,0.0157371373481999));
#24848=CARTESIAN_POINT('Ctrl Pts',(0.649370620646074,-0.571846918937749,
0.0324967135411165));
#24849=CARTESIAN_POINT('Ctrl Pts',(0.647096224417991,-0.559077918077178,
0.0632828231545124));
#24850=CARTESIAN_POINT('Ctrl Pts',(0.645482573914132,-0.549464140887802,
0.077312554408835));
#24851=CARTESIAN_POINT('Ctrl Pts',(0.642442040715078,-0.527312025401873,
0.099464669894764));
#24852=CARTESIAN_POINT('Ctrl Pts',(0.640815160902589,-0.513282519396725,
0.109078032552995));
#24853=CARTESIAN_POINT('Ctrl Pts',(0.63851034608138,-0.482497190457637,
0.121846732641678));
#24854=CARTESIAN_POINT('Ctrl Pts',(0.637867541108654,-0.465737888992352,
0.125));
#24855=CARTESIAN_POINT('Ctrl Pts',(0.637867541108654,-0.45,0.125));
#24856=CARTESIAN_POINT('',(0.65,-0.325,3.9801020972289E-17));
#24857=CARTESIAN_POINT('Ctrl Pts',(0.65,-0.325,6.93889390390723E-18));
#24858=CARTESIAN_POINT('Ctrl Pts',(0.65,-0.325,-0.0157371373481998));
#24859=CARTESIAN_POINT('Ctrl Pts',(0.649370620646074,-0.328153081062251,
-0.0324967135411164));
#24860=CARTESIAN_POINT('Ctrl Pts',(0.647096224417991,-0.340922081922822,
-0.0632828231545123));
#24861=CARTESIAN_POINT('Ctrl Pts',(0.645482573914132,-0.350535859112198,
-0.0773125544088349));
#24862=CARTESIAN_POINT('Ctrl Pts',(0.642442040715078,-0.372687974598127,
-0.0994646698947639));
#24863=CARTESIAN_POINT('Ctrl Pts',(0.640815160902588,-0.386717480603275,
-0.109078032552995));
#24864=CARTESIAN_POINT('Ctrl Pts',(0.63851034608138,-0.417502809542363,
-0.121846732641678));
#24865=CARTESIAN_POINT('Ctrl Pts',(0.637867541108654,-0.434262111007648,
-0.125));
#24866=CARTESIAN_POINT('Ctrl Pts',(0.637867541108654,-0.465737888992352,
-0.125));
#24867=CARTESIAN_POINT('Ctrl Pts',(0.63851034608138,-0.482497190457637,
-0.121846732641678));
#24868=CARTESIAN_POINT('Ctrl Pts',(0.640815160902589,-0.513282519396725,
-0.109078032552995));
#24869=CARTESIAN_POINT('Ctrl Pts',(0.642442040715078,-0.527312025401873,
-0.0994646698947639));
#24870=CARTESIAN_POINT('Ctrl Pts',(0.645482573914132,-0.549464140887802,
-0.0773125544088348));
#24871=CARTESIAN_POINT('Ctrl Pts',(0.647096224417991,-0.559077918077178,
-0.0632828231545123));
#24872=CARTESIAN_POINT('Ctrl Pts',(0.649370620646074,-0.571846918937749,
-0.0324967135411164));
#24873=CARTESIAN_POINT('Ctrl Pts',(0.65,-0.575,-0.0157371373481998));
#24874=CARTESIAN_POINT('Ctrl Pts',(0.65,-0.575,6.24500451351651E-17));
#24875=CARTESIAN_POINT('Ctrl Pts',(0.637867541108654,-0.45,0.125));
#24876=CARTESIAN_POINT('Ctrl Pts',(0.637867541108654,-0.434262111007648,
0.125));
#24877=CARTESIAN_POINT('Ctrl Pts',(0.63851034608138,-0.417502809542363,
0.121846732641678));
#24878=CARTESIAN_POINT('Ctrl Pts',(0.640815160902589,-0.386717480603274,
0.109078032552995));
#24879=CARTESIAN_POINT('Ctrl Pts',(0.642442040715078,-0.372687974598127,
0.0994646698947639));
#24880=CARTESIAN_POINT('Ctrl Pts',(0.645482573914132,-0.350535859112198,
0.0773125544088348));
#24881=CARTESIAN_POINT('Ctrl Pts',(0.647096224417991,-0.340922081922822,
0.0632828231545123));
#24882=CARTESIAN_POINT('Ctrl Pts',(0.649370620646074,-0.328153081062251,
0.0324967135411164));
#24883=CARTESIAN_POINT('Ctrl Pts',(0.65,-0.325,0.0157371373481998));
#24884=CARTESIAN_POINT('Ctrl Pts',(0.65,-0.325,-6.93889390390723E-18));
#24885=CARTESIAN_POINT('Origin',(0.,-0.1,0.));
#24886=CARTESIAN_POINT('',(-0.65,-0.8,7.9602041944578E-17));
#24887=CARTESIAN_POINT('Origin',(0.,-0.8,0.));
#24888=CARTESIAN_POINT('',(-0.65,-0.1,-7.9602041944578E-17));
#24889=CARTESIAN_POINT('',(-0.65,-0.1,7.9602041944578E-17));
#24890=CARTESIAN_POINT('',(-0.65,-0.1,-7.9602041944578E-17));
#24891=CARTESIAN_POINT('Origin',(0.,-0.1,0.));
#24892=CARTESIAN_POINT('',(0.,-0.575,-0.65));
#24893=CARTESIAN_POINT('',(0.,-0.325,-0.65));
#24894=CARTESIAN_POINT('Ctrl Pts',(-1.73472347597681E-17,-0.575,-0.65));
#24895=CARTESIAN_POINT('Ctrl Pts',(0.0157371373481998,-0.575,-0.65));
#24896=CARTESIAN_POINT('Ctrl Pts',(0.0324967135411164,-0.571846918937749,
-0.649370620646074));
#24897=CARTESIAN_POINT('Ctrl Pts',(0.0632828231545123,-0.559077918077178,
-0.647096224417991));
#24898=CARTESIAN_POINT('Ctrl Pts',(0.0773125544088349,-0.549464140887802,
-0.645482573914132));
#24899=CARTESIAN_POINT('Ctrl Pts',(0.099464669894764,-0.527312025401873,
-0.642442040715078));
#24900=CARTESIAN_POINT('Ctrl Pts',(0.109078032552995,-0.513282519396725,
-0.640815160902589));
#24901=CARTESIAN_POINT('Ctrl Pts',(0.121846732641678,-0.482497190457636,
-0.63851034608138));
#24902=CARTESIAN_POINT('Ctrl Pts',(0.125,-0.465737888992352,-0.637867541108654));
#24903=CARTESIAN_POINT('Ctrl Pts',(0.125,-0.434262111007648,-0.637867541108654));
#24904=CARTESIAN_POINT('Ctrl Pts',(0.121846732641678,-0.417502809542364,
-0.63851034608138));
#24905=CARTESIAN_POINT('Ctrl Pts',(0.109078032552995,-0.386717480603275,
-0.640815160902589));
#24906=CARTESIAN_POINT('Ctrl Pts',(0.099464669894764,-0.372687974598127,
-0.642442040715078));
#24907=CARTESIAN_POINT('Ctrl Pts',(0.0773125544088349,-0.350535859112198,
-0.645482573914132));
#24908=CARTESIAN_POINT('Ctrl Pts',(0.0632828231545123,-0.340922081922822,
-0.647096224417991));
#24909=CARTESIAN_POINT('Ctrl Pts',(0.0324967135411164,-0.328153081062251,
-0.649370620646074));
#24910=CARTESIAN_POINT('Ctrl Pts',(0.0157371373481999,-0.325,-0.65));
#24911=CARTESIAN_POINT('Ctrl Pts',(4.5102810375397E-17,-0.325,-0.65));
#24912=CARTESIAN_POINT('',(-0.125,-0.45,-0.637867541108654));
#24913=CARTESIAN_POINT('Ctrl Pts',(4.85722573273506E-17,-0.325,-0.65));
#24914=CARTESIAN_POINT('Ctrl Pts',(-0.0157371373481997,-0.325,-0.65));
#24915=CARTESIAN_POINT('Ctrl Pts',(-0.0324967135411163,-0.328153081062251,
-0.649370620646074));
#24916=CARTESIAN_POINT('Ctrl Pts',(-0.0632828231545122,-0.340922081922822,
-0.647096224417991));
#24917=CARTESIAN_POINT('Ctrl Pts',(-0.0773125544088348,-0.350535859112198,
-0.645482573914132));
#24918=CARTESIAN_POINT('Ctrl Pts',(-0.0994646698947639,-0.372687974598127,
-0.642442040715078));
#24919=CARTESIAN_POINT('Ctrl Pts',(-0.109078032552995,-0.386717480603274,
-0.640815160902589));
#24920=CARTESIAN_POINT('Ctrl Pts',(-0.121846732641678,-0.417502809542363,
-0.63851034608138));
#24921=CARTESIAN_POINT('Ctrl Pts',(-0.125,-0.434262111007648,-0.637867541108654));
#24922=CARTESIAN_POINT('Ctrl Pts',(-0.125,-0.45,-0.637867541108654));
#24923=CARTESIAN_POINT('Ctrl Pts',(-0.125,-0.45,-0.637867541108654));
#24924=CARTESIAN_POINT('Ctrl Pts',(-0.125,-0.465737888992352,-0.637867541108654));
#24925=CARTESIAN_POINT('Ctrl Pts',(-0.121846732641678,-0.482497190457636,
-0.63851034608138));
#24926=CARTESIAN_POINT('Ctrl Pts',(-0.109078032552995,-0.513282519396725,
-0.640815160902589));
#24927=CARTESIAN_POINT('Ctrl Pts',(-0.099464669894764,-0.527312025401873,
-0.642442040715078));
#24928=CARTESIAN_POINT('Ctrl Pts',(-0.0773125544088349,-0.549464140887802,
-0.645482573914132));
#24929=CARTESIAN_POINT('Ctrl Pts',(-0.0632828231545124,-0.559077918077178,
-0.647096224417991));
#24930=CARTESIAN_POINT('Ctrl Pts',(-0.0324967135411165,-0.571846918937749,
-0.649370620646074));
#24931=CARTESIAN_POINT('Ctrl Pts',(-0.0157371373481998,-0.575,-0.65));
#24932=CARTESIAN_POINT('Ctrl Pts',(-1.73472347597681E-17,-0.575,-0.65));
#24933=CARTESIAN_POINT('',(0.,-0.325,0.65));
#24934=CARTESIAN_POINT('',(0.,-0.575,0.65));
#24935=CARTESIAN_POINT('Ctrl Pts',(2.77555756156289E-17,-0.325,0.65));
#24936=CARTESIAN_POINT('Ctrl Pts',(0.0157371373481998,-0.325,0.65));
#24937=CARTESIAN_POINT('Ctrl Pts',(0.0324967135411164,-0.328153081062251,
0.649370620646074));
#24938=CARTESIAN_POINT('Ctrl Pts',(0.0632828231545123,-0.340922081922822,
0.647096224417991));
#24939=CARTESIAN_POINT('Ctrl Pts',(0.0773125544088349,-0.350535859112198,
0.645482573914132));
#24940=CARTESIAN_POINT('Ctrl Pts',(0.099464669894764,-0.372687974598127,
0.642442040715078));
#24941=CARTESIAN_POINT('Ctrl Pts',(0.109078032552995,-0.386717480603275,
0.640815160902589));
#24942=CARTESIAN_POINT('Ctrl Pts',(0.121846732641678,-0.417502809542364,
0.63851034608138));
#24943=CARTESIAN_POINT('Ctrl Pts',(0.125,-0.434262111007648,0.637867541108654));
#24944=CARTESIAN_POINT('Ctrl Pts',(0.125,-0.465737888992352,0.637867541108654));
#24945=CARTESIAN_POINT('Ctrl Pts',(0.121846732641678,-0.482497190457636,
0.63851034608138));
#24946=CARTESIAN_POINT('Ctrl Pts',(0.109078032552995,-0.513282519396725,
0.640815160902589));
#24947=CARTESIAN_POINT('Ctrl Pts',(0.099464669894764,-0.527312025401873,
0.642442040715078));
#24948=CARTESIAN_POINT('Ctrl Pts',(0.077312554408835,-0.549464140887802,
0.645482573914132));
#24949=CARTESIAN_POINT('Ctrl Pts',(0.0632828231545124,-0.559077918077178,
0.647096224417991));
#24950=CARTESIAN_POINT('Ctrl Pts',(0.0324967135411165,-0.571846918937749,
0.649370620646074));
#24951=CARTESIAN_POINT('Ctrl Pts',(0.0157371373481998,-0.575,0.65));
#24952=CARTESIAN_POINT('Ctrl Pts',(-1.38777878078145E-17,-0.575,0.65));
#24953=CARTESIAN_POINT('',(-0.125,-0.45,0.637867541108654));
#24954=CARTESIAN_POINT('Ctrl Pts',(-1.04083408558608E-17,-0.575,0.65));
#24955=CARTESIAN_POINT('Ctrl Pts',(-0.0157371373481998,-0.575,0.65));
#24956=CARTESIAN_POINT('Ctrl Pts',(-0.0324967135411164,-0.571846918937749,
0.649370620646074));
#24957=CARTESIAN_POINT('Ctrl Pts',(-0.0632828231545123,-0.559077918077178,
0.647096224417991));
#24958=CARTESIAN_POINT('Ctrl Pts',(-0.0773125544088349,-0.549464140887802,
0.645482573914132));
#24959=CARTESIAN_POINT('Ctrl Pts',(-0.099464669894764,-0.527312025401873,
0.642442040715078));
#24960=CARTESIAN_POINT('Ctrl Pts',(-0.109078032552995,-0.513282519396725,
0.640815160902589));
#24961=CARTESIAN_POINT('Ctrl Pts',(-0.121846732641678,-0.482497190457636,
0.63851034608138));
#24962=CARTESIAN_POINT('Ctrl Pts',(-0.125,-0.465737888992352,0.637867541108654));
#24963=CARTESIAN_POINT('Ctrl Pts',(-0.125,-0.45,0.637867541108654));
#24964=CARTESIAN_POINT('Ctrl Pts',(-0.125,-0.45,0.637867541108654));
#24965=CARTESIAN_POINT('Ctrl Pts',(-0.125,-0.434262111007648,0.637867541108654));
#24966=CARTESIAN_POINT('Ctrl Pts',(-0.121846732641678,-0.417502809542363,
0.63851034608138));
#24967=CARTESIAN_POINT('Ctrl Pts',(-0.109078032552995,-0.386717480603274,
0.640815160902589));
#24968=CARTESIAN_POINT('Ctrl Pts',(-0.0994646698947639,-0.372687974598127,
0.642442040715078));
#24969=CARTESIAN_POINT('Ctrl Pts',(-0.0773125544088348,-0.350535859112198,
0.645482573914132));
#24970=CARTESIAN_POINT('Ctrl Pts',(-0.0632828231545122,-0.340922081922822,
0.647096224417991));
#24971=CARTESIAN_POINT('Ctrl Pts',(-0.0324967135411163,-0.328153081062251,
0.649370620646074));
#24972=CARTESIAN_POINT('Ctrl Pts',(-0.0157371373481998,-0.325,0.65));
#24973=CARTESIAN_POINT('Ctrl Pts',(4.5102810375397E-17,-0.325,0.65));
#24974=CARTESIAN_POINT('Origin',(0.,-0.45,0.));
#24975=CARTESIAN_POINT('',(-0.125,-0.45,-0.379967103839267));
#24976=CARTESIAN_POINT('',(-0.125,-0.45,0.));
#24977=CARTESIAN_POINT('',(0.125,-0.45,-0.379967103839267));
#24978=CARTESIAN_POINT('Ctrl Pts',(0.125,-0.45,-0.379967103839267));
#24979=CARTESIAN_POINT('Ctrl Pts',(0.125,-0.465813100629203,-0.379967103839267));
#24980=CARTESIAN_POINT('Ctrl Pts',(0.121817958968287,-0.48260129709332,
-0.381057715344782));
#24981=CARTESIAN_POINT('Ctrl Pts',(0.109029967924066,-0.51336346023721,
-0.384911758361269));
#24982=CARTESIAN_POINT('Ctrl Pts',(0.0994291026068839,-0.527347592689753,
-0.38761064154154));
#24983=CARTESIAN_POINT('Ctrl Pts',(0.0773514949786257,-0.549425200318011,
-0.392612801026882));
#24984=CARTESIAN_POINT('Ctrl Pts',(0.0633657881355918,-0.559029081159106,
-0.395252954914593));
#24985=CARTESIAN_POINT('Ctrl Pts',(0.0325978607437828,-0.571819306519379,
-0.398970551469948));
#24986=CARTESIAN_POINT('Ctrl Pts',(0.0158075115832676,-0.575,-0.4));
#24987=CARTESIAN_POINT('Ctrl Pts',(-0.0158075115832676,-0.575,-0.4));
#24988=CARTESIAN_POINT('Ctrl Pts',(-0.0325978607437828,-0.571819306519379,
-0.398970551469948));
#24989=CARTESIAN_POINT('Ctrl Pts',(-0.0633657881355918,-0.559029081159106,
-0.395252954914593));
#24990=CARTESIAN_POINT('Ctrl Pts',(-0.0773514949786256,-0.549425200318011,
-0.392612801026882));
#24991=CARTESIAN_POINT('Ctrl Pts',(-0.0994291026068839,-0.527347592689753,
-0.38761064154154));
#24992=CARTESIAN_POINT('Ctrl Pts',(-0.109029967924066,-0.51336346023721,
-0.384911758361269));
#24993=CARTESIAN_POINT('Ctrl Pts',(-0.121817958968287,-0.48260129709332,
-0.381057715344782));
#24994=CARTESIAN_POINT('Ctrl Pts',(-0.125,-0.465813100629203,-0.379967103839267));
#24995=CARTESIAN_POINT('Ctrl Pts',(-0.125,-0.45,-0.379967103839267));
#24996=CARTESIAN_POINT('Ctrl Pts',(-0.125,-0.45,-0.379967103839267));
#24997=CARTESIAN_POINT('Ctrl Pts',(-0.125,-0.434186899370797,-0.379967103839267));
#24998=CARTESIAN_POINT('Ctrl Pts',(-0.121817958968287,-0.41739870290668,
-0.381057715344782));
#24999=CARTESIAN_POINT('Ctrl Pts',(-0.109029967924066,-0.38663653976279,
-0.384911758361269));
#25000=CARTESIAN_POINT('Ctrl Pts',(-0.0994291026068839,-0.372652407310247,
-0.38761064154154));
#25001=CARTESIAN_POINT('Ctrl Pts',(-0.0773514949786257,-0.350574799681989,
-0.392612801026882));
#25002=CARTESIAN_POINT('Ctrl Pts',(-0.0633657881355918,-0.340970918840894,
-0.395252954914593));
#25003=CARTESIAN_POINT('Ctrl Pts',(-0.0325978607437829,-0.328180693480621,
-0.398970551469948));
#25004=CARTESIAN_POINT('Ctrl Pts',(-0.0158075115832676,-0.325,-0.4));
#25005=CARTESIAN_POINT('Ctrl Pts',(0.0158075115832675,-0.325,-0.4));
#25006=CARTESIAN_POINT('Ctrl Pts',(0.0325978607437828,-0.328180693480621,
-0.398970551469948));
#25007=CARTESIAN_POINT('Ctrl Pts',(0.0633657881355917,-0.340970918840894,
-0.395252954914593));
#25008=CARTESIAN_POINT('Ctrl Pts',(0.0773514949786256,-0.350574799681989,
-0.392612801026882));
#25009=CARTESIAN_POINT('Ctrl Pts',(0.0994291026068839,-0.372652407310247,
-0.38761064154154));
#25010=CARTESIAN_POINT('Ctrl Pts',(0.109029967924066,-0.38663653976279,
-0.384911758361269));
#25011=CARTESIAN_POINT('Ctrl Pts',(0.121817958968287,-0.41739870290668,
-0.381057715344782));
#25012=CARTESIAN_POINT('Ctrl Pts',(0.125,-0.434186899370797,-0.379967103839267));
#25013=CARTESIAN_POINT('Ctrl Pts',(0.125,-0.45,-0.379967103839267));
#25014=CARTESIAN_POINT('Origin',(0.,-0.45,0.));
#25015=CARTESIAN_POINT('',(0.125,-0.45,0.379967103839267));
#25016=CARTESIAN_POINT('',(-0.125,-0.45,0.379967103839267));
#25017=CARTESIAN_POINT('Ctrl Pts',(0.125,-0.45,0.379967103839267));
#25018=CARTESIAN_POINT('Ctrl Pts',(0.125,-0.434186899370797,0.379967103839267));
#25019=CARTESIAN_POINT('Ctrl Pts',(0.121817958968287,-0.41739870290668,
0.381057715344782));
#25020=CARTESIAN_POINT('Ctrl Pts',(0.109029967924066,-0.38663653976279,
0.384911758361269));
#25021=CARTESIAN_POINT('Ctrl Pts',(0.0994291026068839,-0.372652407310247,
0.38761064154154));
#25022=CARTESIAN_POINT('Ctrl Pts',(0.0773514949786256,-0.350574799681989,
0.392612801026882));
#25023=CARTESIAN_POINT('Ctrl Pts',(0.0633657881355918,-0.340970918840894,
0.395252954914593));
#25024=CARTESIAN_POINT('Ctrl Pts',(0.0325978607437828,-0.328180693480621,
0.398970551469948));
#25025=CARTESIAN_POINT('Ctrl Pts',(0.0158075115832676,-0.325,0.4));
#25026=CARTESIAN_POINT('Ctrl Pts',(-0.0158075115832676,-0.325,0.4));
#25027=CARTESIAN_POINT('Ctrl Pts',(-0.0325978607437828,-0.328180693480621,
0.398970551469948));
#25028=CARTESIAN_POINT('Ctrl Pts',(-0.0633657881355918,-0.340970918840894,
0.395252954914593));
#25029=CARTESIAN_POINT('Ctrl Pts',(-0.0773514949786257,-0.350574799681989,
0.392612801026882));
#25030=CARTESIAN_POINT('Ctrl Pts',(-0.0994291026068839,-0.372652407310247,
0.38761064154154));
#25031=CARTESIAN_POINT('Ctrl Pts',(-0.109029967924066,-0.38663653976279,
0.384911758361269));
#25032=CARTESIAN_POINT('Ctrl Pts',(-0.121817958968287,-0.41739870290668,
0.381057715344782));
#25033=CARTESIAN_POINT('Ctrl Pts',(-0.125,-0.434186899370797,0.379967103839267));
#25034=CARTESIAN_POINT('Ctrl Pts',(-0.125,-0.45,0.379967103839267));
#25035=CARTESIAN_POINT('Ctrl Pts',(-0.125,-0.45,0.379967103839267));
#25036=CARTESIAN_POINT('Ctrl Pts',(-0.125,-0.465813100629203,0.379967103839267));
#25037=CARTESIAN_POINT('Ctrl Pts',(-0.121817958968287,-0.48260129709332,
0.381057715344782));
#25038=CARTESIAN_POINT('Ctrl Pts',(-0.109029967924066,-0.51336346023721,
0.384911758361269));
#25039=CARTESIAN_POINT('Ctrl Pts',(-0.0994291026068839,-0.527347592689753,
0.38761064154154));
#25040=CARTESIAN_POINT('Ctrl Pts',(-0.0773514949786256,-0.549425200318011,
0.392612801026882));
#25041=CARTESIAN_POINT('Ctrl Pts',(-0.0633657881355917,-0.559029081159106,
0.395252954914593));
#25042=CARTESIAN_POINT('Ctrl Pts',(-0.0325978607437828,-0.571819306519379,
0.398970551469948));
#25043=CARTESIAN_POINT('Ctrl Pts',(-0.0158075115832675,-0.575,0.4));
#25044=CARTESIAN_POINT('Ctrl Pts',(0.0158075115832676,-0.575,0.4));
#25045=CARTESIAN_POINT('Ctrl Pts',(0.0325978607437828,-0.571819306519379,
0.398970551469948));
#25046=CARTESIAN_POINT('Ctrl Pts',(0.0633657881355917,-0.559029081159106,
0.395252954914593));
#25047=CARTESIAN_POINT('Ctrl Pts',(0.0773514949786257,-0.549425200318011,
0.392612801026882));
#25048=CARTESIAN_POINT('Ctrl Pts',(0.0994291026068839,-0.527347592689753,
0.38761064154154));
#25049=CARTESIAN_POINT('Ctrl Pts',(0.109029967924066,-0.51336346023721,
0.384911758361269));
#25050=CARTESIAN_POINT('Ctrl Pts',(0.121817958968287,-0.48260129709332,
0.381057715344782));
#25051=CARTESIAN_POINT('Ctrl Pts',(0.125,-0.465813100629203,0.379967103839267));
#25052=CARTESIAN_POINT('Ctrl Pts',(0.125,-0.45,0.379967103839267));
#25053=CARTESIAN_POINT('',(-0.125,-0.45,0.));
#25054=CARTESIAN_POINT('Origin',(0.,0.,0.));
#25055=CARTESIAN_POINT('',(-0.4,-0.8,4.89858719658941E-17));
#25056=CARTESIAN_POINT('Origin',(0.,-0.8,0.));
#25057=CARTESIAN_POINT('',(-0.4,0.,4.89858719658941E-17));
#25058=CARTESIAN_POINT('',(-0.4,0.85,-4.89858719658941E-17));
#25059=CARTESIAN_POINT('',(-0.4,0.,4.89858719658941E-17));
#25060=CARTESIAN_POINT('Origin',(0.,0.85,0.));
#25061=CARTESIAN_POINT('Origin',(0.,-0.8,0.));
#25062=CARTESIAN_POINT('Origin',(0.,0.,0.));
#25063=CARTESIAN_POINT('',(-0.8,0.,9.79717439317883E-17));
#25064=CARTESIAN_POINT('Origin',(0.,0.,0.));
#25065=CARTESIAN_POINT('',(0.595438916863769,0.,0.137993139022126));
#25066=CARTESIAN_POINT('',(0.562830534889751,0.,0.238351419397483));
#25067=CARTESIAN_POINT('Origin',(0.562758945330873,0.,0.182851465569258));
#25068=CARTESIAN_POINT('',(0.523653836874034,0.,0.315240018494132));
#25069=CARTESIAN_POINT('Origin',(0.,0.,0.));
#25070=CARTESIAN_POINT('',(0.461629008549572,0.,0.40060987082025));
#25071=CARTESIAN_POINT('Origin',(0.478711351753049,0.,0.347804155687524));
#25072=CARTESIAN_POINT('',(0.40060987082025,0.,0.461629008549572));
#25073=CARTESIAN_POINT('Origin',(0.,0.,0.));
#25074=CARTESIAN_POINT('',(0.315240018494132,0.,0.523653836874034));
#25075=CARTESIAN_POINT('Origin',(0.347804155687523,0.,0.478711351753049));
#25076=CARTESIAN_POINT('',(0.238351419397483,0.,0.562830534889751));
#25077=CARTESIAN_POINT('Origin',(0.,0.,0.));
#25078=CARTESIAN_POINT('',(0.137993139022126,0.,0.595438916863769));
#25079=CARTESIAN_POINT('Origin',(0.182851465569258,0.,0.562758945330873));
#25080=CARTESIAN_POINT('',(0.0527614703521001,0.,0.608938287003997));
#25081=CARTESIAN_POINT('Origin',(0.,0.,0.));
#25082=CARTESIAN_POINT('',(-0.0527614703521003,0.,0.608938287003997));
#25083=CARTESIAN_POINT('Origin',(-1.08697158783324E-16,0.,0.591719772367581));
#25084=CARTESIAN_POINT('',(-0.137993139022126,0.,0.595438916863769));
#25085=CARTESIAN_POINT('Origin',(0.,0.,0.));
#25086=CARTESIAN_POINT('',(-0.238351419397483,0.,0.562830534889751));
#25087=CARTESIAN_POINT('Origin',(-0.182851465569258,0.,0.562758945330873));
#25088=CARTESIAN_POINT('',(-0.315240018494132,0.,0.523653836874034));
#25089=CARTESIAN_POINT('Origin',(0.,0.,0.));
#25090=CARTESIAN_POINT('',(-0.40060987082025,0.,0.461629008549572));
#25091=CARTESIAN_POINT('Origin',(-0.347804155687524,0.,0.478711351753049));
#25092=CARTESIAN_POINT('',(-0.461629008549572,0.,0.40060987082025));
#25093=CARTESIAN_POINT('Origin',(0.,0.,0.));
#25094=CARTESIAN_POINT('',(-0.523653836874034,0.,0.315240018494132));
#25095=CARTESIAN_POINT('Origin',(-0.478711351753049,0.,0.347804155687524));
#25096=CARTESIAN_POINT('',(-0.562830534889751,0.,0.238351419397483));
#25097=CARTESIAN_POINT('Origin',(0.,0.,0.));
#25098=CARTESIAN_POINT('',(-0.595438916863769,0.,0.137993139022126));
#25099=CARTESIAN_POINT('Origin',(-0.562758945330873,0.,0.182851465569258));
#25100=CARTESIAN_POINT('',(-0.608938287003997,0.,0.0527614703521002));
#25101=CARTESIAN_POINT('Origin',(0.,0.,0.));
#25102=CARTESIAN_POINT('',(-0.608938287003997,0.,-0.0527614703521003));
#25103=CARTESIAN_POINT('Origin',(-0.591719772367581,0.,-7.24647725222159E-17));
#25104=CARTESIAN_POINT('',(-0.595438916863769,0.,-0.137993139022126));
#25105=CARTESIAN_POINT('Origin',(0.,0.,0.));
#25106=CARTESIAN_POINT('',(-0.562830534889751,0.,-0.238351419397483));
#25107=CARTESIAN_POINT('Origin',(-0.562758945330873,0.,-0.182851465569258));
#25108=CARTESIAN_POINT('',(-0.523653836874034,0.,-0.315240018494132));
#25109=CARTESIAN_POINT('Origin',(0.,0.,0.));
#25110=CARTESIAN_POINT('',(-0.461629008549572,0.,-0.40060987082025));
#25111=CARTESIAN_POINT('Origin',(-0.478711351753049,0.,-0.347804155687524));
#25112=CARTESIAN_POINT('',(-0.40060987082025,0.,-0.461629008549572));
#25113=CARTESIAN_POINT('Origin',(0.,0.,0.));
#25114=CARTESIAN_POINT('',(-0.315240018494132,0.,-0.523653836874034));
#25115=CARTESIAN_POINT('Origin',(-0.347804155687524,0.,-0.478711351753049));
#25116=CARTESIAN_POINT('',(-0.238351419397483,0.,-0.562830534889751));
#25117=CARTESIAN_POINT('Origin',(0.,0.,0.));
#25118=CARTESIAN_POINT('',(-0.137993139022126,0.,-0.595438916863769));
#25119=CARTESIAN_POINT('Origin',(-0.182851465569258,0.,-0.562758945330873));
#25120=CARTESIAN_POINT('',(-0.0527614703521002,0.,-0.608938287003997));
#25121=CARTESIAN_POINT('Origin',(0.,0.,0.));
#25122=CARTESIAN_POINT('',(0.0527614703521003,0.,-0.608938287003997));
#25123=CARTESIAN_POINT('Origin',(3.6232386261108E-17,0.,-0.591719772367581));
#25124=CARTESIAN_POINT('',(0.137993139022126,0.,-0.595438916863769));
#25125=CARTESIAN_POINT('Origin',(0.,0.,0.));
#25126=CARTESIAN_POINT('',(0.238351419397483,0.,-0.562830534889751));
#25127=CARTESIAN_POINT('Origin',(0.182851465569258,0.,-0.562758945330873));
#25128=CARTESIAN_POINT('',(0.315240018494132,0.,-0.523653836874034));
#25129=CARTESIAN_POINT('Origin',(0.,0.,0.));
#25130=CARTESIAN_POINT('',(0.40060987082025,0.,-0.461629008549572));
#25131=CARTESIAN_POINT('Origin',(0.347804155687524,0.,-0.478711351753049));
#25132=CARTESIAN_POINT('',(0.461629008549572,0.,-0.40060987082025));
#25133=CARTESIAN_POINT('Origin',(0.,0.,0.));
#25134=CARTESIAN_POINT('',(0.523653836874034,0.,-0.315240018494132));
#25135=CARTESIAN_POINT('Origin',(0.478711351753049,0.,-0.347804155687524));
#25136=CARTESIAN_POINT('',(0.562830534889751,0.,-0.238351419397483));
#25137=CARTESIAN_POINT('Origin',(0.,0.,0.));
#25138=CARTESIAN_POINT('',(0.595438916863769,0.,-0.137993139022126));
#25139=CARTESIAN_POINT('Origin',(0.562758945330873,0.,-0.182851465569258));
#25140=CARTESIAN_POINT('',(0.608938287003997,0.,-0.0527614703521001));
#25141=CARTESIAN_POINT('Origin',(0.,0.,0.));
#25142=CARTESIAN_POINT('',(0.608938287003997,0.,0.0527614703521001));
#25143=CARTESIAN_POINT('Origin',(0.591719772367581,0.,0.));
#25144=CARTESIAN_POINT('Origin',(0.,0.,0.));
#25145=CARTESIAN_POINT('Origin',(0.,0.,0.));
#25146=CARTESIAN_POINT('',(-0.8,-0.1,9.79717439317883E-17));
#25147=CARTESIAN_POINT('Origin',(0.,-0.1,0.));
#25148=CARTESIAN_POINT('',(-0.8,0.,-9.79717439317883E-17));
#25149=CARTESIAN_POINT('Origin',(0.,-0.1,0.));
#25150=CARTESIAN_POINT('Origin',(0.,0.75,0.));
#25151=CARTESIAN_POINT('',(-0.8,0.75,9.79717439317883E-17));
#25152=CARTESIAN_POINT('Origin',(0.,0.75,0.));
#25153=CARTESIAN_POINT('',(0.562830534889751,0.75,0.238351419397483));
#25154=CARTESIAN_POINT('',(0.595438916863769,0.75,0.137993139022126));
#25155=CARTESIAN_POINT('Origin',(0.562758945330873,0.75,0.182851465569258));
#25156=CARTESIAN_POINT('',(0.608938287003997,0.75,0.0527614703521002));
#25157=CARTESIAN_POINT('Origin',(0.,0.75,0.));
#25158=CARTESIAN_POINT('',(0.608938287003997,0.75,-0.0527614703521002));
#25159=CARTESIAN_POINT('Origin',(0.591719772367581,0.75,0.));
#25160=CARTESIAN_POINT('',(0.595438916863769,0.75,-0.137993139022126));
#25161=CARTESIAN_POINT('Origin',(0.,0.75,0.));
#25162=CARTESIAN_POINT('',(0.562830534889751,0.75,-0.238351419397483));
#25163=CARTESIAN_POINT('Origin',(0.562758945330873,0.75,-0.182851465569258));
#25164=CARTESIAN_POINT('',(0.523653836874034,0.75,-0.315240018494132));
#25165=CARTESIAN_POINT('Origin',(0.,0.75,0.));
#25166=CARTESIAN_POINT('',(0.461629008549572,0.75,-0.40060987082025));
#25167=CARTESIAN_POINT('Origin',(0.478711351753049,0.75,-0.347804155687524));
#25168=CARTESIAN_POINT('',(0.40060987082025,0.75,-0.461629008549572));
#25169=CARTESIAN_POINT('Origin',(0.,0.75,0.));
#25170=CARTESIAN_POINT('',(0.315240018494132,0.75,-0.523653836874034));
#25171=CARTESIAN_POINT('Origin',(0.347804155687524,0.75,-0.478711351753049));
#25172=CARTESIAN_POINT('',(0.238351419397483,0.75,-0.562830534889751));
#25173=CARTESIAN_POINT('Origin',(0.,0.75,0.));
#25174=CARTESIAN_POINT('',(0.137993139022126,0.75,-0.595438916863769));
#25175=CARTESIAN_POINT('Origin',(0.182851465569258,0.75,-0.562758945330873));
#25176=CARTESIAN_POINT('',(0.0527614703521003,0.75,-0.608938287003997));
#25177=CARTESIAN_POINT('Origin',(0.,0.75,0.));
#25178=CARTESIAN_POINT('',(-0.0527614703521002,0.75,-0.608938287003997));
#25179=CARTESIAN_POINT('Origin',(3.6232386261108E-17,0.75,-0.591719772367581));
#25180=CARTESIAN_POINT('',(-0.137993139022126,0.75,-0.595438916863769));
#25181=CARTESIAN_POINT('Origin',(0.,0.75,0.));
#25182=CARTESIAN_POINT('',(-0.238351419397483,0.75,-0.562830534889751));
#25183=CARTESIAN_POINT('Origin',(-0.182851465569258,0.75,-0.562758945330873));
#25184=CARTESIAN_POINT('',(-0.315240018494132,0.75,-0.523653836874034));
#25185=CARTESIAN_POINT('Origin',(0.,0.75,0.));
#25186=CARTESIAN_POINT('',(-0.40060987082025,0.75,-0.461629008549572));
#25187=CARTESIAN_POINT('Origin',(-0.347804155687524,0.75,-0.478711351753049));
#25188=CARTESIAN_POINT('',(-0.461629008549572,0.75,-0.40060987082025));
#25189=CARTESIAN_POINT('Origin',(0.,0.75,0.));
#25190=CARTESIAN_POINT('',(-0.523653836874034,0.75,-0.315240018494132));
#25191=CARTESIAN_POINT('Origin',(-0.478711351753049,0.75,-0.347804155687524));
#25192=CARTESIAN_POINT('',(-0.562830534889751,0.75,-0.238351419397483));
#25193=CARTESIAN_POINT('Origin',(0.,0.75,0.));
#25194=CARTESIAN_POINT('',(-0.595438916863769,0.75,-0.137993139022126));
#25195=CARTESIAN_POINT('Origin',(-0.562758945330873,0.75,-0.182851465569258));
#25196=CARTESIAN_POINT('',(-0.608938287003997,0.75,-0.0527614703521003));
#25197=CARTESIAN_POINT('Origin',(0.,0.75,0.));
#25198=CARTESIAN_POINT('',(-0.608938287003997,0.75,0.0527614703521002));
#25199=CARTESIAN_POINT('Origin',(-0.591719772367581,0.75,-7.24647725222159E-17));
#25200=CARTESIAN_POINT('',(-0.595438916863769,0.75,0.137993139022126));
#25201=CARTESIAN_POINT('Origin',(0.,0.75,0.));
#25202=CARTESIAN_POINT('',(-0.562830534889751,0.75,0.238351419397483));
#25203=CARTESIAN_POINT('Origin',(-0.562758945330873,0.75,0.182851465569258));
#25204=CARTESIAN_POINT('',(-0.523653836874034,0.75,0.315240018494132));
#25205=CARTESIAN_POINT('Origin',(0.,0.75,0.));
#25206=CARTESIAN_POINT('',(-0.461629008549572,0.75,0.40060987082025));
#25207=CARTESIAN_POINT('Origin',(-0.478711351753049,0.75,0.347804155687524));
#25208=CARTESIAN_POINT('',(-0.40060987082025,0.75,0.461629008549572));
#25209=CARTESIAN_POINT('Origin',(0.,0.75,0.));
#25210=CARTESIAN_POINT('',(-0.315240018494132,0.75,0.523653836874034));
#25211=CARTESIAN_POINT('Origin',(-0.347804155687524,0.75,0.478711351753049));
#25212=CARTESIAN_POINT('',(-0.238351419397483,0.75,0.562830534889751));
#25213=CARTESIAN_POINT('Origin',(0.,0.75,0.));
#25214=CARTESIAN_POINT('',(-0.137993139022126,0.75,0.595438916863769));
#25215=CARTESIAN_POINT('Origin',(-0.182851465569258,0.75,0.562758945330873));
#25216=CARTESIAN_POINT('',(-0.0527614703521003,0.75,0.608938287003997));
#25217=CARTESIAN_POINT('Origin',(0.,0.75,0.));
#25218=CARTESIAN_POINT('',(0.0527614703521001,0.75,0.608938287003997));
#25219=CARTESIAN_POINT('Origin',(-1.08697158783324E-16,0.75,0.591719772367581));
#25220=CARTESIAN_POINT('',(0.137993139022126,0.75,0.595438916863769));
#25221=CARTESIAN_POINT('Origin',(0.,0.75,0.));
#25222=CARTESIAN_POINT('',(0.238351419397483,0.75,0.562830534889751));
#25223=CARTESIAN_POINT('Origin',(0.182851465569258,0.75,0.562758945330873));
#25224=CARTESIAN_POINT('',(0.315240018494132,0.75,0.523653836874034));
#25225=CARTESIAN_POINT('Origin',(0.,0.75,0.));
#25226=CARTESIAN_POINT('',(0.40060987082025,0.75,0.461629008549572));
#25227=CARTESIAN_POINT('Origin',(0.347804155687523,0.75,0.478711351753049));
#25228=CARTESIAN_POINT('',(0.461629008549572,0.75,0.40060987082025));
#25229=CARTESIAN_POINT('Origin',(0.,0.75,0.));
#25230=CARTESIAN_POINT('',(0.523653836874034,0.75,0.315240018494132));
#25231=CARTESIAN_POINT('Origin',(0.478711351753049,0.75,0.347804155687524));
#25232=CARTESIAN_POINT('Origin',(0.,0.75,0.));
#25233=CARTESIAN_POINT('Origin',(0.,0.75,0.));
#25234=CARTESIAN_POINT('',(-0.8,0.85,9.79717439317883E-17));
#25235=CARTESIAN_POINT('Origin',(0.,0.85,0.));
#25236=CARTESIAN_POINT('',(-0.8,0.75,9.79717439317883E-17));
#25237=CARTESIAN_POINT('Origin',(0.,0.85,0.));
#25238=CARTESIAN_POINT('Origin',(0.562758945330873,0.,0.182851465569258));
#25239=CARTESIAN_POINT('',(0.595438916863769,0.,0.137993139022126));
#25240=CARTESIAN_POINT('',(0.562830534889751,0.,0.238351419397483));
#25241=CARTESIAN_POINT('Origin',(0.,0.,0.));
#25242=CARTESIAN_POINT('',(0.523653836874034,0.,0.315240018494132));
#25243=CARTESIAN_POINT('Origin',(0.478711351753049,0.,0.347804155687524));
#25244=CARTESIAN_POINT('',(0.461629008549572,0.,0.40060987082025));
#25245=CARTESIAN_POINT('Origin',(0.,0.,0.));
#25246=CARTESIAN_POINT('',(0.40060987082025,0.,0.461629008549572));
#25247=CARTESIAN_POINT('Origin',(0.347804155687523,0.,0.478711351753049));
#25248=CARTESIAN_POINT('',(0.315240018494132,0.,0.523653836874034));
#25249=CARTESIAN_POINT('Origin',(0.,0.,0.));
#25250=CARTESIAN_POINT('',(0.238351419397483,0.,0.562830534889751));
#25251=CARTESIAN_POINT('Origin',(0.182851465569258,0.,0.562758945330873));
#25252=CARTESIAN_POINT('',(0.137993139022126,0.,0.595438916863769));
#25253=CARTESIAN_POINT('Origin',(0.,0.,0.));
#25254=CARTESIAN_POINT('',(0.0527614703521,0.,0.608938287003997));
#25255=CARTESIAN_POINT('Origin',(-1.08697158783324E-16,0.,0.591719772367581));
#25256=CARTESIAN_POINT('',(-0.0527614703521002,0.,0.608938287003997));
#25257=CARTESIAN_POINT('Origin',(0.,0.,0.));
#25258=CARTESIAN_POINT('',(-0.137993139022126,0.,0.595438916863769));
#25259=CARTESIAN_POINT('Origin',(-0.182851465569258,0.,0.562758945330873));
#25260=CARTESIAN_POINT('',(-0.238351419397483,0.,0.562830534889751));
#25261=CARTESIAN_POINT('Origin',(0.,0.,0.));
#25262=CARTESIAN_POINT('',(-0.315240018494132,0.,0.523653836874034));
#25263=CARTESIAN_POINT('Origin',(-0.347804155687524,0.,0.478711351753049));
#25264=CARTESIAN_POINT('',(-0.40060987082025,0.,0.461629008549572));
#25265=CARTESIAN_POINT('Origin',(0.,0.,0.));
#25266=CARTESIAN_POINT('',(-0.461629008549572,0.,0.40060987082025));
#25267=CARTESIAN_POINT('Origin',(-0.478711351753049,0.,0.347804155687524));
#25268=CARTESIAN_POINT('',(-0.523653836874034,0.,0.315240018494132));
#25269=CARTESIAN_POINT('Origin',(0.,0.,0.));
#25270=CARTESIAN_POINT('',(-0.562830534889751,0.,0.238351419397483));
#25271=CARTESIAN_POINT('Origin',(-0.562758945330873,0.,0.182851465569258));
#25272=CARTESIAN_POINT('',(-0.595438916863769,0.,0.137993139022126));
#25273=CARTESIAN_POINT('Origin',(0.,0.,0.));
#25274=CARTESIAN_POINT('',(-0.608938287003997,0.,0.0527614703521));
#25275=CARTESIAN_POINT('Origin',(-0.591719772367581,0.,-7.24647725222159E-17));
#25276=CARTESIAN_POINT('',(-0.608938287003997,0.,-0.0527614703521002));
#25277=CARTESIAN_POINT('Origin',(0.,0.,0.));
#25278=CARTESIAN_POINT('',(-0.595438916863769,0.,-0.137993139022126));
#25279=CARTESIAN_POINT('Origin',(-0.562758945330873,0.,-0.182851465569258));
#25280=CARTESIAN_POINT('',(-0.562830534889751,0.,-0.238351419397483));
#25281=CARTESIAN_POINT('Origin',(0.,0.,0.));
#25282=CARTESIAN_POINT('',(-0.523653836874034,0.,-0.315240018494132));
#25283=CARTESIAN_POINT('Origin',(-0.478711351753049,0.,-0.347804155687524));
#25284=CARTESIAN_POINT('',(-0.461629008549572,0.,-0.40060987082025));
#25285=CARTESIAN_POINT('Origin',(0.,0.,0.));
#25286=CARTESIAN_POINT('',(-0.40060987082025,0.,-0.461629008549572));
#25287=CARTESIAN_POINT('Origin',(-0.347804155687524,0.,-0.478711351753049));
#25288=CARTESIAN_POINT('',(-0.315240018494132,0.,-0.523653836874034));
#25289=CARTESIAN_POINT('Origin',(0.,0.,0.));
#25290=CARTESIAN_POINT('',(-0.238351419397483,0.,-0.562830534889751));
#25291=CARTESIAN_POINT('Origin',(-0.182851465569258,0.,-0.562758945330873));
#25292=CARTESIAN_POINT('',(-0.137993139022126,0.,-0.595438916863769));
#25293=CARTESIAN_POINT('Origin',(0.,0.,0.));
#25294=CARTESIAN_POINT('',(-0.0527614703521,0.,-0.608938287003997));
#25295=CARTESIAN_POINT('Origin',(3.6232386261108E-17,0.,-0.591719772367581));
#25296=CARTESIAN_POINT('',(0.0527614703521001,0.,-0.608938287003997));
#25297=CARTESIAN_POINT('Origin',(0.,0.,0.));
#25298=CARTESIAN_POINT('',(0.137993139022126,0.,-0.595438916863769));
#25299=CARTESIAN_POINT('Origin',(0.182851465569258,0.,-0.562758945330873));
#25300=CARTESIAN_POINT('',(0.238351419397483,0.,-0.562830534889751));
#25301=CARTESIAN_POINT('Origin',(0.,0.,0.));
#25302=CARTESIAN_POINT('',(0.315240018494132,0.,-0.523653836874034));
#25303=CARTESIAN_POINT('Origin',(0.347804155687524,0.,-0.478711351753049));
#25304=CARTESIAN_POINT('',(0.40060987082025,0.,-0.461629008549572));
#25305=CARTESIAN_POINT('Origin',(0.,0.,0.));
#25306=CARTESIAN_POINT('',(0.461629008549572,0.,-0.40060987082025));
#25307=CARTESIAN_POINT('Origin',(0.478711351753049,0.,-0.347804155687524));
#25308=CARTESIAN_POINT('',(0.523653836874034,0.,-0.315240018494132));
#25309=CARTESIAN_POINT('Origin',(0.,0.,0.));
#25310=CARTESIAN_POINT('',(0.562830534889751,0.,-0.238351419397483));
#25311=CARTESIAN_POINT('Origin',(0.562758945330873,0.,-0.182851465569258));
#25312=CARTESIAN_POINT('',(0.595438916863769,0.,-0.137993139022126));
#25313=CARTESIAN_POINT('Origin',(0.,0.,0.));
#25314=CARTESIAN_POINT('',(0.608938287003997,0.,0.0527614703521001));
#25315=CARTESIAN_POINT('Origin',(0.591719772367581,0.,0.));
#25316=CARTESIAN_POINT('',(0.608938287003997,0.,-0.0527614703521001));
#25317=CARTESIAN_POINT('Origin',(0.,0.,0.));
#25318=CARTESIAN_POINT('',(0.,0.,0.));
#25319=CARTESIAN_POINT('',(0.,0.,0.));
#25320=CARTESIAN_POINT('Origin',(6.97091003018116,2.1,7.));
#25321=CARTESIAN_POINT('',(5.97091003018116,2.1,7.));
#25322=CARTESIAN_POINT('Origin',(6.97091003018116,2.1,7.));
#25323=CARTESIAN_POINT('',(6.17091003018116,2.1,7.));
#25324=CARTESIAN_POINT('Origin',(6.97091003018116,2.1,7.));
#25325=CARTESIAN_POINT('Origin',(6.97091003018116,2.1,7.));
#25326=CARTESIAN_POINT('',(5.97091003018116,43.3,7.));
#25327=CARTESIAN_POINT('Origin',(6.97091003018116,43.3,7.));
#25328=CARTESIAN_POINT('',(5.97091003018116,2.1,7.));
#25329=CARTESIAN_POINT('Origin',(6.97091003018116,43.3,7.));
#25330=CARTESIAN_POINT('Origin',(6.97091003018116,-5.1,7.));
#25331=CARTESIAN_POINT('',(6.80591003018116,-5.,7.));
#25332=CARTESIAN_POINT('Origin',(6.97091003018116,-5.,7.));
#25333=CARTESIAN_POINT('',(6.80591003018116,-3.4,7.));
#25334=CARTESIAN_POINT('',(6.80591003018116,-5.1,7.));
#25335=CARTESIAN_POINT('Origin',(6.97091003018116,-3.4,7.));
#25336=CARTESIAN_POINT('Origin',(6.97091003018116,-3.4,7.));
#25337=CARTESIAN_POINT('Origin',(6.97091003018116,1.4,7.));
#25338=CARTESIAN_POINT('',(6.17091003018116,1.4,7.));
#25339=CARTESIAN_POINT('Origin',(6.97091003018116,1.4,7.));
#25340=CARTESIAN_POINT('',(6.37091003018116,1.4,7.));
#25341=CARTESIAN_POINT('Origin',(6.97091003018116,1.4,7.));
#25342=CARTESIAN_POINT('Origin',(6.97091003018116,1.4,7.));
#25343=CARTESIAN_POINT('',(6.17091003018116,1.4,7.));
#25344=CARTESIAN_POINT('Origin',(6.97091003018116,-1.8,7.));
#25345=CARTESIAN_POINT('',(6.37091003018116,-5.,7.));
#25346=CARTESIAN_POINT('',(6.37091003018116,-1.8,7.));
#25347=CARTESIAN_POINT('Origin',(6.97091003018116,-5.,7.));
#25348=CARTESIAN_POINT('Origin',(6.97091003018116,-5.,7.));
#25349=CARTESIAN_POINT('',(0.,0.,0.));
#25350=CARTESIAN_POINT('Origin',(6.97091003018116,-2.65,7.));
#25351=CARTESIAN_POINT('',(6.36591003018116,-1.4,7.));
#25352=CARTESIAN_POINT('Origin',(6.97091003018116,-1.4,7.));
#25353=CARTESIAN_POINT('',(6.36591003018116,-2.65,7.));
#25354=CARTESIAN_POINT('',(6.36591003018116,-2.65,7.));
#25355=CARTESIAN_POINT('Origin',(6.97091003018116,-2.65,7.));
#25356=CARTESIAN_POINT('Origin',(6.97091003018116,-2.65,7.));
#25357=CARTESIAN_POINT('',(6.17091003018116,-1.4,7.));
#25358=CARTESIAN_POINT('Origin',(6.97091003018116,-1.4,7.));
#25359=CARTESIAN_POINT('',(6.17091003018116,-2.65,7.));
#25360=CARTESIAN_POINT('',(6.17091003018116,-2.65,7.));
#25361=CARTESIAN_POINT('Origin',(6.97091003018116,-2.65,7.));
#25362=CARTESIAN_POINT('Origin',(6.97091003018116,-1.4,7.));
#25363=CARTESIAN_POINT('Origin',(6.97091003018116,-2.65,7.));
#25364=CARTESIAN_POINT('',(0.,0.,0.));
#25365=CARTESIAN_POINT('Origin',(6.97091003018116,-0.4,7.));
#25366=CARTESIAN_POINT('',(6.36591003018116,0.4,7.));
#25367=CARTESIAN_POINT('Origin',(6.97091003018116,0.4,7.));
#25368=CARTESIAN_POINT('',(6.36591003018116,-0.4,7.));
#25369=CARTESIAN_POINT('',(6.36591003018116,-0.4,7.));
#25370=CARTESIAN_POINT('Origin',(6.97091003018116,-0.4,7.));
#25371=CARTESIAN_POINT('Origin',(6.97091003018116,-0.4,7.));
#25372=CARTESIAN_POINT('',(6.17091003018116,0.4,7.));
#25373=CARTESIAN_POINT('Origin',(6.97091003018116,0.4,7.));
#25374=CARTESIAN_POINT('',(6.17091003018116,-0.4,7.));
#25375=CARTESIAN_POINT('',(6.17091003018116,-0.4,7.));
#25376=CARTESIAN_POINT('Origin',(6.97091003018116,-0.4,7.));
#25377=CARTESIAN_POINT('Origin',(6.97091003018116,0.4,7.));
#25378=CARTESIAN_POINT('Origin',(6.97091003018116,-0.4,7.));
#25379=CARTESIAN_POINT('',(0.,0.,0.));
#25380=CARTESIAN_POINT('Origin',(6.97091003018116,-4.,6.));
#25381=CARTESIAN_POINT('',(6.82091003018116,-4.,6.4));
#25382=CARTESIAN_POINT('Origin',(6.97091003018116,-4.,6.4));
#25383=CARTESIAN_POINT('',(6.82091003018116,-4.,6.));
#25384=CARTESIAN_POINT('',(6.82091003018116,-4.,6.));
#25385=CARTESIAN_POINT('Origin',(6.97091003018116,-4.,6.));
#25386=CARTESIAN_POINT('Origin',(6.97091003018116,-4.,6.4));
#25387=CARTESIAN_POINT('Origin',(6.97091003018116,-4.,6.));
#25388=CARTESIAN_POINT('',(0.,0.,0.));
#25389=CARTESIAN_POINT('Origin',(6.97091003018116,-4.,7.6));
#25390=CARTESIAN_POINT('',(6.82091003018116,-4.,8.));
#25391=CARTESIAN_POINT('Origin',(6.97091003018116,-4.,8.));
#25392=CARTESIAN_POINT('',(6.82091003018116,-4.,7.6));
#25393=CARTESIAN_POINT('',(6.82091003018116,-4.,7.6));
#25394=CARTESIAN_POINT('Origin',(6.97091003018116,-4.,7.6));
#25395=CARTESIAN_POINT('Origin',(6.97091003018116,-4.,8.));
#25396=CARTESIAN_POINT('Origin',(6.97091003018116,-4.,7.6));
#25397=CARTESIAN_POINT('',(0.,0.,0.));
#25398=CARTESIAN_POINT('Origin',(6.97091003018116,-5.2,7.));
#25399=CARTESIAN_POINT('',(6.74591003018116,-5.,7.));
#25400=CARTESIAN_POINT('Origin',(6.97091003018116,-5.,7.));
#25401=CARTESIAN_POINT('',(6.74591003018116,-5.2,7.));
#25402=CARTESIAN_POINT('',(6.74591003018116,-5.2,7.));
#25403=CARTESIAN_POINT('Origin',(6.97091003018116,-5.2,7.));
#25404=CARTESIAN_POINT('Origin',(6.97091003018116,-5.2,7.));
#25405=CARTESIAN_POINT('',(6.17091003018116,-5.,7.));
#25406=CARTESIAN_POINT('Origin',(6.97091003018116,-5.,7.));
#25407=CARTESIAN_POINT('',(6.17091003018116,-5.2,7.));
#25408=CARTESIAN_POINT('',(6.17091003018116,-5.2,7.));
#25409=CARTESIAN_POINT('Origin',(6.97091003018116,-5.2,7.));
#25410=CARTESIAN_POINT('Origin',(6.97091003018116,-5.,7.));
#25411=CARTESIAN_POINT('Origin',(6.97091003018116,-5.2,7.));
#25412=CARTESIAN_POINT('',(0.,0.,0.));
#25413=CARTESIAN_POINT('Origin',(6.97091003018116,2.75,7.99));
#25414=CARTESIAN_POINT('',(7.14389846910121,2.63094119100208,7.99));
#25415=CARTESIAN_POINT('',(7.14389846910121,2.86905880899792,7.99));
#25416=CARTESIAN_POINT('',(7.14389846910121,2.35,7.99));
#25417=CARTESIAN_POINT('Origin',(6.97091003018116,2.75,7.99));
#25418=CARTESIAN_POINT('Origin',(6.97091003018116,2.75,7.99));
#25419=CARTESIAN_POINT('',(6.7979215912611,2.63094119100208,7.99));
#25420=CARTESIAN_POINT('Ctrl Pts',(6.7979215912611,2.63094119100208,7.99));
#25421=CARTESIAN_POINT('Ctrl Pts',(6.80531516486984,2.62019857760471,7.99129192197638));
#25422=CARTESIAN_POINT('Ctrl Pts',(6.81361289145555,2.61031229062726,7.99265394943905));
#25423=CARTESIAN_POINT('Ctrl Pts',(6.84101795633608,2.58290722574673,7.9967480843909));
#25424=CARTESIAN_POINT('Ctrl Pts',(6.86457986242187,2.56675794366705,7.99969589327638));
#25425=CARTESIAN_POINT('Ctrl Pts',(6.91629712554874,2.54530220603509,8.00385029472357));
#25426=CARTESIAN_POINT('Ctrl Pts',(6.9444587993513,2.54,8.005));
#25427=CARTESIAN_POINT('Ctrl Pts',(6.99736126101101,2.54,8.005));
#25428=CARTESIAN_POINT('Ctrl Pts',(7.02552293481357,2.54530220603509,8.00385029472357));
#25429=CARTESIAN_POINT('Ctrl Pts',(7.07724019794044,2.56675794366705,7.99969589327638));
#25430=CARTESIAN_POINT('Ctrl Pts',(7.10080210402623,2.58290722574673,7.9967480843909));
#25431=CARTESIAN_POINT('Ctrl Pts',(7.12820716890676,2.61031229062726,7.99265394943905));
#25432=CARTESIAN_POINT('Ctrl Pts',(7.13650489549247,2.62019857760471,7.99129192197638));
#25433=CARTESIAN_POINT('Ctrl Pts',(7.14389846910121,2.63094119100208,7.99));
#25434=CARTESIAN_POINT('',(6.76091003018116,2.75,7.99));
#25435=CARTESIAN_POINT('Origin',(6.97091003018116,2.75,7.99));
#25436=CARTESIAN_POINT('',(6.76091003018116,2.75,8.48522725533839));
#25437=CARTESIAN_POINT('',(6.76091003018116,2.75,7.99));
#25438=CARTESIAN_POINT('',(7.18091003018116,2.75,8.48522725533839));
#25439=CARTESIAN_POINT('Ctrl Pts',(7.18091003018116,2.75,8.48522725533839));
#25440=CARTESIAN_POINT('Ctrl Pts',(7.18091003018116,2.72359447307555,8.48522725533839));
#25441=CARTESIAN_POINT('Ctrl Pts',(7.17562576745075,2.69545292590929,8.48600415954412));
#25442=CARTESIAN_POINT('Ctrl Pts',(7.15418379321749,2.64372373109487,8.48880073282317));
#25443=CARTESIAN_POINT('Ctrl Pts',(7.13802795415155,2.62013307587204,8.49077897157582));
#25444=CARTESIAN_POINT('Ctrl Pts',(7.10077720006852,2.58288232178902,8.49448481141327));
#25445=CARTESIAN_POINT('Ctrl Pts',(7.07718643848692,2.56672628999865,8.49645455657129));
#25446=CARTESIAN_POINT('Ctrl Pts',(7.02545688158706,2.54528417517378,8.49923165515645));
#25447=CARTESIAN_POINT('Ctrl Pts',(6.99731520869044,2.54,8.5));
#25448=CARTESIAN_POINT('Ctrl Pts',(6.94450485167187,2.54,8.5));
#25449=CARTESIAN_POINT('Ctrl Pts',(6.91636317877526,2.54528417517378,8.49923165515645));
#25450=CARTESIAN_POINT('Ctrl Pts',(6.86463362187539,2.56672628999865,8.49645455657129));
#25451=CARTESIAN_POINT('Ctrl Pts',(6.84104286029379,2.58288232178902,8.49448481141327));
#25452=CARTESIAN_POINT('Ctrl Pts',(6.80379210621076,2.62013307587204,8.49077897157582));
#25453=CARTESIAN_POINT('Ctrl Pts',(6.78763626714482,2.64372373109487,8.48880073282317));
#25454=CARTESIAN_POINT('Ctrl Pts',(6.76619429291156,2.69545292590929,8.48600415954412));
#25455=CARTESIAN_POINT('Ctrl Pts',(6.76091003018116,2.72359447307555,8.48522725533839));
#25456=CARTESIAN_POINT('Ctrl Pts',(6.76091003018116,2.75,8.48522725533839));
#25457=CARTESIAN_POINT('Ctrl Pts',(6.76091003018116,2.75,8.48522725533839));
#25458=CARTESIAN_POINT('Ctrl Pts',(6.76091003018116,2.77640552692445,8.48522725533839));
#25459=CARTESIAN_POINT('Ctrl Pts',(6.76619429291156,2.80454707409071,8.48600415954412));
#25460=CARTESIAN_POINT('Ctrl Pts',(6.78763626714482,2.85627626890513,8.48880073282317));
#25461=CARTESIAN_POINT('Ctrl Pts',(6.80379210621076,2.87986692412796,8.49077897157582));
#25462=CARTESIAN_POINT('Ctrl Pts',(6.84104286029379,2.91711767821098,8.49448481141327));
#25463=CARTESIAN_POINT('Ctrl Pts',(6.86463362187539,2.93327371000135,8.49645455657129));
#25464=CARTESIAN_POINT('Ctrl Pts',(6.91636317877526,2.95471582482622,8.49923165515645));
#25465=CARTESIAN_POINT('Ctrl Pts',(6.94450485167187,2.96,8.5));
#25466=CARTESIAN_POINT('Ctrl Pts',(6.99731520869044,2.96,8.5));
#25467=CARTESIAN_POINT('Ctrl Pts',(7.02545688158706,2.95471582482622,8.49923165515645));
#25468=CARTESIAN_POINT('Ctrl Pts',(7.07718643848692,2.93327371000135,8.49645455657129));
#25469=CARTESIAN_POINT('Ctrl Pts',(7.10077720006852,2.91711767821098,8.49448481141327));
#25470=CARTESIAN_POINT('Ctrl Pts',(7.13802795415155,2.87986692412796,8.49077897157582));
#25471=CARTESIAN_POINT('Ctrl Pts',(7.15418379321749,2.85627626890513,8.48880073282317));
#25472=CARTESIAN_POINT('Ctrl Pts',(7.17562576745075,2.80454707409071,8.48600415954412));
#25473=CARTESIAN_POINT('Ctrl Pts',(7.18091003018116,2.77640552692445,8.48522725533839));
#25474=CARTESIAN_POINT('Ctrl Pts',(7.18091003018116,2.75,8.48522725533839));
#25475=CARTESIAN_POINT('',(6.7979215912611,2.86905880899792,7.99));
#25476=CARTESIAN_POINT('Origin',(6.97091003018116,2.75,7.99));
#25477=CARTESIAN_POINT('Ctrl Pts',(7.14389846910121,2.86905880899792,7.99));
#25478=CARTESIAN_POINT('Ctrl Pts',(7.13650489549247,2.87980142239529,7.99129192197638));
#25479=CARTESIAN_POINT('Ctrl Pts',(7.12820716890676,2.88968770937274,7.99265394943905));
#25480=CARTESIAN_POINT('Ctrl Pts',(7.10080210402623,2.91709277425327,7.9967480843909));
#25481=CARTESIAN_POINT('Ctrl Pts',(7.07724019794044,2.93324205633295,7.99969589327638));
#25482=CARTESIAN_POINT('Ctrl Pts',(7.02552293481357,2.95469779396491,8.00385029472357));
#25483=CARTESIAN_POINT('Ctrl Pts',(6.99736126101101,2.96,8.005));
#25484=CARTESIAN_POINT('Ctrl Pts',(6.9444587993513,2.96,8.005));
#25485=CARTESIAN_POINT('Ctrl Pts',(6.91629712554875,2.95469779396491,8.00385029472357));
#25486=CARTESIAN_POINT('Ctrl Pts',(6.86457986242187,2.93324205633295,7.99969589327638));
#25487=CARTESIAN_POINT('Ctrl Pts',(6.84101795633608,2.91709277425327,7.9967480843909));
#25488=CARTESIAN_POINT('Ctrl Pts',(6.81361289145555,2.88968770937274,7.99265394943905));
#25489=CARTESIAN_POINT('Ctrl Pts',(6.80531516486984,2.87980142239529,7.99129192197638));
#25490=CARTESIAN_POINT('Ctrl Pts',(6.7979215912611,2.86905880899792,7.99));
#25491=CARTESIAN_POINT('Origin',(6.97091003018116,2.75,7.99));
#25492=CARTESIAN_POINT('',(6.7979215912611,2.35,7.99));
#25493=CARTESIAN_POINT('Origin',(6.97091003018116,2.35,7.));
#25494=CARTESIAN_POINT('',(5.96591003018116,3.15,7.));
#25495=CARTESIAN_POINT('Origin',(6.97091003018116,3.15,7.));
#25496=CARTESIAN_POINT('',(5.96591003018116,2.35,7.));
#25497=CARTESIAN_POINT('',(5.96591003018116,2.35,7.));
#25498=CARTESIAN_POINT('Origin',(6.97091003018116,2.35,7.));
#25499=CARTESIAN_POINT('Origin',(6.97091003018116,2.35,7.));
#25500=CARTESIAN_POINT('',(5.47091003018116,3.15,7.));
#25501=CARTESIAN_POINT('Origin',(6.97091003018116,3.15,7.));
#25502=CARTESIAN_POINT('',(5.47091003018116,2.35,7.));
#25503=CARTESIAN_POINT('',(5.47091003018116,2.35,7.));
#25504=CARTESIAN_POINT('Origin',(6.97091003018116,2.35,7.));
#25505=CARTESIAN_POINT('Origin',(6.97091003018116,3.15,7.));
#25506=CARTESIAN_POINT('Origin',(6.97091003018116,2.35,7.));
#25507=CARTESIAN_POINT('',(0.,0.,0.));
#25508=CARTESIAN_POINT('Origin',(6.97091003018116,42.85,7.99));
#25509=CARTESIAN_POINT('',(7.14389846910121,42.7309411910021,7.99));
#25510=CARTESIAN_POINT('',(7.14389846910121,42.9690588089979,7.99));
#25511=CARTESIAN_POINT('',(7.14389846910121,42.45,7.99));
#25512=CARTESIAN_POINT('Origin',(6.97091003018116,42.85,7.99));
#25513=CARTESIAN_POINT('Origin',(6.97091003018116,42.85,7.99));
#25514=CARTESIAN_POINT('',(6.7979215912611,42.7309411910021,7.99));
#25515=CARTESIAN_POINT('Ctrl Pts',(6.7979215912611,42.7309411910021,7.99));
#25516=CARTESIAN_POINT('Ctrl Pts',(6.80531516486984,42.7201985776047,7.99129192197638));
#25517=CARTESIAN_POINT('Ctrl Pts',(6.81361289145555,42.7103122906273,7.99265394943905));
#25518=CARTESIAN_POINT('Ctrl Pts',(6.84101795633608,42.6829072257467,7.9967480843909));
#25519=CARTESIAN_POINT('Ctrl Pts',(6.86457986242187,42.6667579436671,7.99969589327637));
#25520=CARTESIAN_POINT('Ctrl Pts',(6.91629712554875,42.6453022060351,8.00385029472357));
#25521=CARTESIAN_POINT('Ctrl Pts',(6.9444587993513,42.64,8.005));
#25522=CARTESIAN_POINT('Ctrl Pts',(6.99736126101101,42.64,8.005));
#25523=CARTESIAN_POINT('Ctrl Pts',(7.02552293481356,42.6453022060351,8.00385029472357));
#25524=CARTESIAN_POINT('Ctrl Pts',(7.07724019794044,42.6667579436671,7.99969589327638));
#25525=CARTESIAN_POINT('Ctrl Pts',(7.10080210402623,42.6829072257467,7.9967480843909));
#25526=CARTESIAN_POINT('Ctrl Pts',(7.12820716890676,42.7103122906273,7.99265394943905));
#25527=CARTESIAN_POINT('Ctrl Pts',(7.13650489549247,42.7201985776047,7.99129192197638));
#25528=CARTESIAN_POINT('Ctrl Pts',(7.14389846910121,42.7309411910021,7.99));
#25529=CARTESIAN_POINT('',(6.76091003018116,42.85,7.99));
#25530=CARTESIAN_POINT('Origin',(6.97091003018116,42.85,7.99));
#25531=CARTESIAN_POINT('',(6.76091003018116,42.85,8.48522725533839));
#25532=CARTESIAN_POINT('',(6.76091003018116,42.85,7.99));
#25533=CARTESIAN_POINT('',(7.18091003018116,42.85,8.48522725533839));
#25534=CARTESIAN_POINT('Ctrl Pts',(7.18091003018116,42.85,8.48522725533839));
#25535=CARTESIAN_POINT('Ctrl Pts',(7.18091003018116,42.8235944730755,8.48522725533839));
#25536=CARTESIAN_POINT('Ctrl Pts',(7.17562576745075,42.7954529259093,8.48600415954412));
#25537=CARTESIAN_POINT('Ctrl Pts',(7.15418379321749,42.7437237310949,8.48880073282317));
#25538=CARTESIAN_POINT('Ctrl Pts',(7.13802795415155,42.720133075872,8.49077897157582));
#25539=CARTESIAN_POINT('Ctrl Pts',(7.10077720006852,42.682882321789,8.49448481141327));
#25540=CARTESIAN_POINT('Ctrl Pts',(7.07718643848692,42.6667262899986,8.49645455657129));
#25541=CARTESIAN_POINT('Ctrl Pts',(7.02545688158705,42.6452841751738,8.49923165515646));
#25542=CARTESIAN_POINT('Ctrl Pts',(6.99731520869044,42.64,8.5));
#25543=CARTESIAN_POINT('Ctrl Pts',(6.94450485167187,42.64,8.5));
#25544=CARTESIAN_POINT('Ctrl Pts',(6.91636317877526,42.6452841751738,8.49923165515646));
#25545=CARTESIAN_POINT('Ctrl Pts',(6.86463362187539,42.6667262899986,8.49645455657129));
#25546=CARTESIAN_POINT('Ctrl Pts',(6.84104286029379,42.682882321789,8.49448481141327));
#25547=CARTESIAN_POINT('Ctrl Pts',(6.80379210621076,42.720133075872,8.49077897157582));
#25548=CARTESIAN_POINT('Ctrl Pts',(6.78763626714482,42.7437237310949,8.48880073282317));
#25549=CARTESIAN_POINT('Ctrl Pts',(6.76619429291156,42.7954529259093,8.48600415954412));
#25550=CARTESIAN_POINT('Ctrl Pts',(6.76091003018116,42.8235944730756,8.48522725533839));
#25551=CARTESIAN_POINT('Ctrl Pts',(6.76091003018116,42.85,8.48522725533839));
#25552=CARTESIAN_POINT('Ctrl Pts',(6.76091003018116,42.85,8.48522725533839));
#25553=CARTESIAN_POINT('Ctrl Pts',(6.76091003018116,42.8764055269245,8.48522725533839));
#25554=CARTESIAN_POINT('Ctrl Pts',(6.76619429291156,42.9045470740907,8.48600415954412));
#25555=CARTESIAN_POINT('Ctrl Pts',(6.78763626714482,42.9562762689051,8.48880073282317));
#25556=CARTESIAN_POINT('Ctrl Pts',(6.80379210621076,42.979866924128,8.49077897157582));
#25557=CARTESIAN_POINT('Ctrl Pts',(6.84104286029379,43.017117678211,8.49448481141327));
#25558=CARTESIAN_POINT('Ctrl Pts',(6.86463362187539,43.0332737100014,8.49645455657129));
#25559=CARTESIAN_POINT('Ctrl Pts',(6.91636317877526,43.0547158248262,8.49923165515646));
#25560=CARTESIAN_POINT('Ctrl Pts',(6.94450485167187,43.06,8.5));
#25561=CARTESIAN_POINT('Ctrl Pts',(6.99731520869044,43.06,8.5));
#25562=CARTESIAN_POINT('Ctrl Pts',(7.02545688158705,43.0547158248262,8.49923165515646));
#25563=CARTESIAN_POINT('Ctrl Pts',(7.07718643848692,43.0332737100014,8.49645455657129));
#25564=CARTESIAN_POINT('Ctrl Pts',(7.10077720006852,43.017117678211,8.49448481141327));
#25565=CARTESIAN_POINT('Ctrl Pts',(7.13802795415155,42.979866924128,8.49077897157582));
#25566=CARTESIAN_POINT('Ctrl Pts',(7.15418379321749,42.9562762689051,8.48880073282317));
#25567=CARTESIAN_POINT('Ctrl Pts',(7.17562576745075,42.9045470740907,8.48600415954412));
#25568=CARTESIAN_POINT('Ctrl Pts',(7.18091003018116,42.8764055269245,8.48522725533839));
#25569=CARTESIAN_POINT('Ctrl Pts',(7.18091003018116,42.85,8.48522725533839));
#25570=CARTESIAN_POINT('',(6.7979215912611,42.9690588089979,7.99));
#25571=CARTESIAN_POINT('Origin',(6.97091003018116,42.85,7.99));
#25572=CARTESIAN_POINT('Ctrl Pts',(7.14389846910122,42.9690588089979,7.99));
#25573=CARTESIAN_POINT('Ctrl Pts',(7.13650489549248,42.9798014223953,7.99129192197638));
#25574=CARTESIAN_POINT('Ctrl Pts',(7.12820716890676,42.9896877093727,7.99265394943905));
#25575=CARTESIAN_POINT('Ctrl Pts',(7.10080210402623,43.0170927742533,7.9967480843909));
#25576=CARTESIAN_POINT('Ctrl Pts',(7.07724019794044,43.033242056333,7.99969589327637));
#25577=CARTESIAN_POINT('Ctrl Pts',(7.02552293481357,43.0546977939649,8.00385029472357));
#25578=CARTESIAN_POINT('Ctrl Pts',(6.99736126101101,43.06,8.005));
#25579=CARTESIAN_POINT('Ctrl Pts',(6.9444587993513,43.06,8.005));
#25580=CARTESIAN_POINT('Ctrl Pts',(6.91629712554875,43.0546977939649,8.00385029472357));
#25581=CARTESIAN_POINT('Ctrl Pts',(6.86457986242187,43.033242056333,7.99969589327637));
#25582=CARTESIAN_POINT('Ctrl Pts',(6.84101795633608,43.0170927742533,7.9967480843909));
#25583=CARTESIAN_POINT('Ctrl Pts',(6.81361289145555,42.9896877093727,7.99265394943905));
#25584=CARTESIAN_POINT('Ctrl Pts',(6.80531516486984,42.9798014223953,7.99129192197638));
#25585=CARTESIAN_POINT('Ctrl Pts',(6.7979215912611,42.9690588089979,7.99));
#25586=CARTESIAN_POINT('Origin',(6.97091003018116,42.85,7.99));
#25587=CARTESIAN_POINT('',(6.7979215912611,42.45,7.99));
#25588=CARTESIAN_POINT('Origin',(6.97091003018116,42.45,7.));
#25589=CARTESIAN_POINT('',(5.96591003018116,43.25,7.));
#25590=CARTESIAN_POINT('Origin',(6.97091003018116,43.25,7.));
#25591=CARTESIAN_POINT('',(5.96591003018116,42.45,7.));
#25592=CARTESIAN_POINT('',(5.96591003018116,42.45,7.));
#25593=CARTESIAN_POINT('Origin',(6.97091003018116,42.45,7.));
#25594=CARTESIAN_POINT('Origin',(6.97091003018116,42.45,7.));
#25595=CARTESIAN_POINT('',(5.47091003018116,43.25,7.));
#25596=CARTESIAN_POINT('Origin',(6.97091003018116,43.25,7.));
#25597=CARTESIAN_POINT('',(5.47091003018116,42.45,7.));
#25598=CARTESIAN_POINT('',(5.47091003018116,42.45,7.));
#25599=CARTESIAN_POINT('Origin',(6.97091003018116,42.45,7.));
#25600=CARTESIAN_POINT('Origin',(6.97091003018116,43.25,7.));
#25601=CARTESIAN_POINT('Origin',(6.97091003018116,42.45,7.));
#25602=CARTESIAN_POINT('',(0.,0.,0.));
#25603=CARTESIAN_POINT('Origin',(6.97091003018116,7.,7.));
#25604=CARTESIAN_POINT('',(3.37091003018116,37.,7.));
#25605=CARTESIAN_POINT('Origin',(6.97091003018116,37.,7.));
#25606=CARTESIAN_POINT('',(3.37091003018116,7.,7.));
#25607=CARTESIAN_POINT('',(3.37091003018116,7.,7.));
#25608=CARTESIAN_POINT('Origin',(6.97091003018116,7.,7.));
#25609=CARTESIAN_POINT('Origin',(6.97091003018116,7.,7.));
#25610=CARTESIAN_POINT('',(2.97091003018116,37.,7.));
#25611=CARTESIAN_POINT('Origin',(6.97091003018116,37.,7.));
#25612=CARTESIAN_POINT('',(2.97091003018116,7.,7.));
#25613=CARTESIAN_POINT('',(2.97091003018116,7.,7.));
#25614=CARTESIAN_POINT('Origin',(6.97091003018116,7.,7.));
#25615=CARTESIAN_POINT('Origin',(6.97091003018116,37.,7.));
#25616=CARTESIAN_POINT('Origin',(6.97091003018116,7.,7.));
#25617=CARTESIAN_POINT('',(0.,0.,0.));
#25618=CARTESIAN_POINT('Origin',(6.97091003018116,6.6,7.));
#25619=CARTESIAN_POINT('',(5.96591003018116,7.,7.));
#25620=CARTESIAN_POINT('Origin',(6.97091003018116,7.,7.));
#25621=CARTESIAN_POINT('',(5.96591003018116,6.6,7.));
#25622=CARTESIAN_POINT('',(5.96591003018116,6.6,7.));
#25623=CARTESIAN_POINT('Origin',(6.97091003018116,6.6,7.));
#25624=CARTESIAN_POINT('Origin',(6.97091003018116,6.6,7.));
#25625=CARTESIAN_POINT('',(2.97091003018116,7.,7.));
#25626=CARTESIAN_POINT('Origin',(6.97091003018116,7.,7.));
#25627=CARTESIAN_POINT('',(2.97091003018116,6.6,7.));
#25628=CARTESIAN_POINT('',(2.97091003018116,6.6,7.));
#25629=CARTESIAN_POINT('Origin',(6.97091003018116,6.6,7.));
#25630=CARTESIAN_POINT('Origin',(6.97091003018116,7.,7.));
#25631=CARTESIAN_POINT('Origin',(6.97091003018116,6.6,7.));
#25632=CARTESIAN_POINT('',(0.,0.,0.));
#25633=CARTESIAN_POINT('Origin',(6.97091003018116,37.,7.));
#25634=CARTESIAN_POINT('',(5.96591003018116,37.4,7.));
#25635=CARTESIAN_POINT('Origin',(6.97091003018116,37.4,7.));
#25636=CARTESIAN_POINT('',(5.96591003018116,37.,7.));
#25637=CARTESIAN_POINT('',(5.96591003018116,37.,7.));
#25638=CARTESIAN_POINT('Origin',(6.97091003018116,37.,7.));
#25639=CARTESIAN_POINT('Origin',(6.97091003018116,37.,7.));
#25640=CARTESIAN_POINT('',(2.97091003018116,37.4,7.));
#25641=CARTESIAN_POINT('Origin',(6.97091003018116,37.4,7.));
#25642=CARTESIAN_POINT('',(2.97091003018116,37.,7.));
#25643=CARTESIAN_POINT('',(2.97091003018116,37.,7.));
#25644=CARTESIAN_POINT('Origin',(6.97091003018116,37.,7.));
#25645=CARTESIAN_POINT('Origin',(6.97091003018116,37.4,7.));
#25646=CARTESIAN_POINT('Origin',(6.97091003018116,37.,7.));
#25647=CARTESIAN_POINT('',(0.,0.,0.));
#25648=CARTESIAN_POINT('Origin',(6.97091003018116,7.6,7.99));
#25649=CARTESIAN_POINT('',(7.14389846910121,7.48094119100208,7.99));
#25650=CARTESIAN_POINT('',(7.14389846910121,7.71905880899792,7.99));
#25651=CARTESIAN_POINT('',(7.14389846910121,7.,7.99));
#25652=CARTESIAN_POINT('Origin',(6.97091003018116,7.6,7.99));
#25653=CARTESIAN_POINT('Origin',(6.97091003018116,7.6,7.99));
#25654=CARTESIAN_POINT('',(6.7979215912611,7.48094119100208,7.99));
#25655=CARTESIAN_POINT('Ctrl Pts',(6.7979215912611,7.48094119100208,7.99));
#25656=CARTESIAN_POINT('Ctrl Pts',(6.80531516486984,7.47019857760471,7.99129192197638));
#25657=CARTESIAN_POINT('Ctrl Pts',(6.81361289145555,7.46031229062725,7.99265394943905));
#25658=CARTESIAN_POINT('Ctrl Pts',(6.84101795633608,7.43290722574673,7.9967480843909));
#25659=CARTESIAN_POINT('Ctrl Pts',(6.86457986242187,7.41675794366705,7.99969589327638));
#25660=CARTESIAN_POINT('Ctrl Pts',(6.91629712554875,7.39530220603509,8.00385029472357));
#25661=CARTESIAN_POINT('Ctrl Pts',(6.9444587993513,7.39,8.005));
#25662=CARTESIAN_POINT('Ctrl Pts',(6.99736126101101,7.39,8.005));
#25663=CARTESIAN_POINT('Ctrl Pts',(7.02552293481356,7.39530220603509,8.00385029472357));
#25664=CARTESIAN_POINT('Ctrl Pts',(7.07724019794044,7.41675794366705,7.99969589327638));
#25665=CARTESIAN_POINT('Ctrl Pts',(7.10080210402623,7.43290722574673,7.9967480843909));
#25666=CARTESIAN_POINT('Ctrl Pts',(7.12820716890676,7.46031229062725,7.99265394943905));
#25667=CARTESIAN_POINT('Ctrl Pts',(7.13650489549247,7.47019857760471,7.99129192197638));
#25668=CARTESIAN_POINT('Ctrl Pts',(7.14389846910121,7.48094119100208,7.99));
#25669=CARTESIAN_POINT('',(6.76091003018116,7.6,7.99));
#25670=CARTESIAN_POINT('Origin',(6.97091003018116,7.6,7.99));
#25671=CARTESIAN_POINT('',(6.76091003018116,7.6,8.78770802985275));
#25672=CARTESIAN_POINT('',(6.76091003018116,7.6,7.99));
#25673=CARTESIAN_POINT('',(7.18091003018116,7.6,8.78770802985275));
#25674=CARTESIAN_POINT('Ctrl Pts',(7.18091003018116,7.6,8.78770802985275));
#25675=CARTESIAN_POINT('Ctrl Pts',(7.18091003018116,7.57360603148425,8.78770802985275));
#25676=CARTESIAN_POINT('Ctrl Pts',(7.17563026313288,7.54546934556601,8.78835284034214));
#25677=CARTESIAN_POINT('Ctrl Pts',(7.15419155416006,7.49373688397397,8.79067700538683));
#25678=CARTESIAN_POINT('Ctrl Pts',(7.13803391906352,7.47013904078401,8.79232226897314));
#25679=CARTESIAN_POINT('Ctrl Pts',(7.10077110728482,7.43287622900531,8.79540680803063));
#25680=CARTESIAN_POINT('Ctrl Pts',(7.07717321270923,7.4167185016358,8.79704717240673));
#25681=CARTESIAN_POINT('Ctrl Pts',(7.02544057769236,7.39527972468261,8.79936011492601));
#25682=CARTESIAN_POINT('Ctrl Pts',(6.9973038316932,7.39,8.8));
#25683=CARTESIAN_POINT('Ctrl Pts',(6.94451622866912,7.39,8.8));
#25684=CARTESIAN_POINT('Ctrl Pts',(6.91637948266995,7.39527972468261,8.79936011492601));
#25685=CARTESIAN_POINT('Ctrl Pts',(6.86464684765309,7.4167185016358,8.79704717240673));
#25686=CARTESIAN_POINT('Ctrl Pts',(6.84104895307749,7.43287622900531,8.79540680803063));
#25687=CARTESIAN_POINT('Ctrl Pts',(6.80378614129879,7.47013904078401,8.79232226897314));
#25688=CARTESIAN_POINT('Ctrl Pts',(6.78762850620226,7.49373688397397,8.79067700538683));
#25689=CARTESIAN_POINT('Ctrl Pts',(6.76618979722943,7.54546934556601,8.78835284034214));
#25690=CARTESIAN_POINT('Ctrl Pts',(6.76091003018116,7.57360603148426,8.78770802985275));
#25691=CARTESIAN_POINT('Ctrl Pts',(6.76091003018116,7.6,8.78770802985275));
#25692=CARTESIAN_POINT('Ctrl Pts',(6.76091003018116,7.6,8.78770802985275));
#25693=CARTESIAN_POINT('Ctrl Pts',(6.76091003018116,7.62639396851575,8.78770802985275));
#25694=CARTESIAN_POINT('Ctrl Pts',(6.76618979722943,7.65453065443399,8.78835284034214));
#25695=CARTESIAN_POINT('Ctrl Pts',(6.78762850620226,7.70626311602603,8.79067700538683));
#25696=CARTESIAN_POINT('Ctrl Pts',(6.80378614129879,7.72986095921599,8.79232226897314));
#25697=CARTESIAN_POINT('Ctrl Pts',(6.84104895307749,7.76712377099468,8.79540680803063));
#25698=CARTESIAN_POINT('Ctrl Pts',(6.86464684765309,7.78328149836419,8.79704717240673));
#25699=CARTESIAN_POINT('Ctrl Pts',(6.91637948266995,7.80472027531739,8.79936011492601));
#25700=CARTESIAN_POINT('Ctrl Pts',(6.94451622866912,7.81,8.8));
#25701=CARTESIAN_POINT('Ctrl Pts',(6.9973038316932,7.81,8.8));
#25702=CARTESIAN_POINT('Ctrl Pts',(7.02544057769236,7.80472027531739,8.79936011492601));
#25703=CARTESIAN_POINT('Ctrl Pts',(7.07717321270923,7.7832814983642,8.79704717240673));
#25704=CARTESIAN_POINT('Ctrl Pts',(7.10077110728482,7.76712377099468,8.79540680803063));
#25705=CARTESIAN_POINT('Ctrl Pts',(7.13803391906352,7.72986095921599,8.79232226897314));
#25706=CARTESIAN_POINT('Ctrl Pts',(7.15419155416005,7.70626311602603,8.79067700538683));
#25707=CARTESIAN_POINT('Ctrl Pts',(7.17563026313288,7.65453065443398,8.78835284034214));
#25708=CARTESIAN_POINT('Ctrl Pts',(7.18091003018116,7.62639396851574,8.78770802985275));
#25709=CARTESIAN_POINT('Ctrl Pts',(7.18091003018116,7.6,8.78770802985275));
#25710=CARTESIAN_POINT('',(6.7979215912611,7.71905880899792,7.99));
#25711=CARTESIAN_POINT('Origin',(6.97091003018116,7.6,7.99));
#25712=CARTESIAN_POINT('Ctrl Pts',(7.14389846910121,7.71905880899792,7.99));
#25713=CARTESIAN_POINT('Ctrl Pts',(7.13650489549247,7.72980142239529,7.99129192197638));
#25714=CARTESIAN_POINT('Ctrl Pts',(7.12820716890676,7.73968770937274,7.99265394943905));
#25715=CARTESIAN_POINT('Ctrl Pts',(7.10080210402623,7.76709277425327,7.9967480843909));
#25716=CARTESIAN_POINT('Ctrl Pts',(7.07724019794044,7.78324205633295,7.99969589327638));
#25717=CARTESIAN_POINT('Ctrl Pts',(7.02552293481356,7.80469779396491,8.00385029472357));
#25718=CARTESIAN_POINT('Ctrl Pts',(6.99736126101101,7.81,8.005));
#25719=CARTESIAN_POINT('Ctrl Pts',(6.9444587993513,7.81,8.005));
#25720=CARTESIAN_POINT('Ctrl Pts',(6.91629712554875,7.80469779396491,8.00385029472357));
#25721=CARTESIAN_POINT('Ctrl Pts',(6.86457986242187,7.78324205633295,7.99969589327638));
#25722=CARTESIAN_POINT('Ctrl Pts',(6.84101795633608,7.76709277425327,7.9967480843909));
#25723=CARTESIAN_POINT('Ctrl Pts',(6.81361289145555,7.73968770937274,7.99265394943905));
#25724=CARTESIAN_POINT('Ctrl Pts',(6.80531516486984,7.72980142239529,7.99129192197638));
#25725=CARTESIAN_POINT('Ctrl Pts',(6.7979215912611,7.71905880899792,7.99));
#25726=CARTESIAN_POINT('Origin',(6.97091003018116,7.6,7.99));
#25727=CARTESIAN_POINT('',(6.7979215912611,7.,7.99));
#25728=CARTESIAN_POINT('Origin',(6.97091003018116,7.,7.));
#25729=CARTESIAN_POINT('',(5.96591003018116,8.2,7.));
#25730=CARTESIAN_POINT('Origin',(6.97091003018116,8.2,7.));
#25731=CARTESIAN_POINT('',(5.96591003018116,7.,7.));
#25732=CARTESIAN_POINT('',(5.96591003018116,7.,7.));
#25733=CARTESIAN_POINT('Origin',(6.97091003018116,7.,7.));
#25734=CARTESIAN_POINT('Origin',(6.97091003018116,7.,7.));
#25735=CARTESIAN_POINT('',(5.17091003018116,8.2,7.));
#25736=CARTESIAN_POINT('Origin',(6.97091003018116,8.2,7.));
#25737=CARTESIAN_POINT('',(5.17091003018116,7.,7.));
#25738=CARTESIAN_POINT('',(5.17091003018116,7.,7.));
#25739=CARTESIAN_POINT('Origin',(6.97091003018116,7.,7.));
#25740=CARTESIAN_POINT('Origin',(6.97091003018116,8.2,7.));
#25741=CARTESIAN_POINT('Origin',(6.97091003018116,7.,7.));
#25742=CARTESIAN_POINT('',(0.,0.,0.));
#25743=CARTESIAN_POINT('Origin',(6.97091003018116,36.4,7.99));
#25744=CARTESIAN_POINT('',(7.14389846910121,36.2809411910021,7.99));
#25745=CARTESIAN_POINT('',(7.14389846910121,36.5190588089979,7.99));
#25746=CARTESIAN_POINT('',(7.14389846910121,35.8,7.99));
#25747=CARTESIAN_POINT('Origin',(6.97091003018116,36.4,7.99));
#25748=CARTESIAN_POINT('Origin',(6.97091003018116,36.4,7.99));
#25749=CARTESIAN_POINT('',(6.7979215912611,36.2809411910021,7.99));
#25750=CARTESIAN_POINT('Ctrl Pts',(6.7979215912611,36.2809411910021,7.99));
#25751=CARTESIAN_POINT('Ctrl Pts',(6.80531516486984,36.2701985776047,7.99129192197638));
#25752=CARTESIAN_POINT('Ctrl Pts',(6.81361289145555,36.2603122906273,7.99265394943905));
#25753=CARTESIAN_POINT('Ctrl Pts',(6.84101795633608,36.2329072257467,7.9967480843909));
#25754=CARTESIAN_POINT('Ctrl Pts',(6.86457986242187,36.216757943667,7.99969589327637));
#25755=CARTESIAN_POINT('Ctrl Pts',(6.91629712554875,36.1953022060351,8.00385029472357));
#25756=CARTESIAN_POINT('Ctrl Pts',(6.9444587993513,36.19,8.005));
#25757=CARTESIAN_POINT('Ctrl Pts',(6.99736126101101,36.19,8.005));
#25758=CARTESIAN_POINT('Ctrl Pts',(7.02552293481357,36.1953022060351,8.00385029472357));
#25759=CARTESIAN_POINT('Ctrl Pts',(7.07724019794044,36.216757943667,7.99969589327637));
#25760=CARTESIAN_POINT('Ctrl Pts',(7.10080210402623,36.2329072257467,7.9967480843909));
#25761=CARTESIAN_POINT('Ctrl Pts',(7.12820716890676,36.2603122906273,7.99265394943905));
#25762=CARTESIAN_POINT('Ctrl Pts',(7.13650489549247,36.2701985776047,7.99129192197638));
#25763=CARTESIAN_POINT('Ctrl Pts',(7.14389846910121,36.2809411910021,7.99));
#25764=CARTESIAN_POINT('',(6.76091003018116,36.4,7.99));
#25765=CARTESIAN_POINT('Origin',(6.97091003018116,36.4,7.99));
#25766=CARTESIAN_POINT('',(6.76091003018116,36.4,8.78770802985275));
#25767=CARTESIAN_POINT('',(6.76091003018116,36.4,7.99));
#25768=CARTESIAN_POINT('',(7.18091003018116,36.4,8.78770802985275));
#25769=CARTESIAN_POINT('Ctrl Pts',(7.18091003018116,36.4,8.78770802985275));
#25770=CARTESIAN_POINT('Ctrl Pts',(7.18091003018116,36.3736060314843,8.78770802985275));
#25771=CARTESIAN_POINT('Ctrl Pts',(7.17563026313289,36.345469345566,8.78835284034214));
#25772=CARTESIAN_POINT('Ctrl Pts',(7.15419155416006,36.293736883974,8.79067700538683));
#25773=CARTESIAN_POINT('Ctrl Pts',(7.13803391906352,36.270139040784,8.79232226897314));
#25774=CARTESIAN_POINT('Ctrl Pts',(7.10077110728482,36.2328762290053,8.79540680803063));
#25775=CARTESIAN_POINT('Ctrl Pts',(7.07717321270923,36.2167185016358,8.79704717240673));
#25776=CARTESIAN_POINT('Ctrl Pts',(7.02544057769236,36.1952797246826,8.79936011492601));
#25777=CARTESIAN_POINT('Ctrl Pts',(6.9973038316932,36.19,8.8));
#25778=CARTESIAN_POINT('Ctrl Pts',(6.94451622866912,36.19,8.8));
#25779=CARTESIAN_POINT('Ctrl Pts',(6.91637948266995,36.1952797246826,8.79936011492601));
#25780=CARTESIAN_POINT('Ctrl Pts',(6.86464684765309,36.2167185016358,8.79704717240673));
#25781=CARTESIAN_POINT('Ctrl Pts',(6.84104895307749,36.2328762290053,8.79540680803063));
#25782=CARTESIAN_POINT('Ctrl Pts',(6.80378614129879,36.270139040784,8.79232226897314));
#25783=CARTESIAN_POINT('Ctrl Pts',(6.78762850620225,36.293736883974,8.79067700538683));
#25784=CARTESIAN_POINT('Ctrl Pts',(6.76618979722943,36.345469345566,8.78835284034214));
#25785=CARTESIAN_POINT('Ctrl Pts',(6.76091003018116,36.3736060314843,8.78770802985275));
#25786=CARTESIAN_POINT('Ctrl Pts',(6.76091003018116,36.4,8.78770802985275));
#25787=CARTESIAN_POINT('Ctrl Pts',(6.76091003018116,36.4,8.78770802985275));
#25788=CARTESIAN_POINT('Ctrl Pts',(6.76091003018116,36.4263939685157,8.78770802985275));
#25789=CARTESIAN_POINT('Ctrl Pts',(6.76618979722943,36.454530654434,8.78835284034214));
#25790=CARTESIAN_POINT('Ctrl Pts',(6.78762850620225,36.506263116026,8.79067700538683));
#25791=CARTESIAN_POINT('Ctrl Pts',(6.80378614129879,36.529860959216,8.79232226897314));
#25792=CARTESIAN_POINT('Ctrl Pts',(6.84104895307749,36.5671237709947,8.79540680803063));
#25793=CARTESIAN_POINT('Ctrl Pts',(6.86464684765309,36.5832814983642,8.79704717240673));
#25794=CARTESIAN_POINT('Ctrl Pts',(6.91637948266995,36.6047202753174,8.79936011492601));
#25795=CARTESIAN_POINT('Ctrl Pts',(6.94451622866912,36.61,8.8));
#25796=CARTESIAN_POINT('Ctrl Pts',(6.9973038316932,36.61,8.8));
#25797=CARTESIAN_POINT('Ctrl Pts',(7.02544057769236,36.6047202753174,8.79936011492601));
#25798=CARTESIAN_POINT('Ctrl Pts',(7.07717321270923,36.5832814983642,8.79704717240673));
#25799=CARTESIAN_POINT('Ctrl Pts',(7.10077110728482,36.5671237709947,8.79540680803063));
#25800=CARTESIAN_POINT('Ctrl Pts',(7.13803391906352,36.529860959216,8.79232226897314));
#25801=CARTESIAN_POINT('Ctrl Pts',(7.15419155416006,36.506263116026,8.79067700538683));
#25802=CARTESIAN_POINT('Ctrl Pts',(7.17563026313288,36.454530654434,8.78835284034214));
#25803=CARTESIAN_POINT('Ctrl Pts',(7.18091003018116,36.4263939685157,8.78770802985275));
#25804=CARTESIAN_POINT('Ctrl Pts',(7.18091003018116,36.4,8.78770802985275));
#25805=CARTESIAN_POINT('',(6.7979215912611,36.5190588089979,7.99));
#25806=CARTESIAN_POINT('Origin',(6.97091003018116,36.4,7.99));
#25807=CARTESIAN_POINT('Ctrl Pts',(7.14389846910122,36.5190588089979,7.99));
#25808=CARTESIAN_POINT('Ctrl Pts',(7.13650489549247,36.5298014223953,7.99129192197638));
#25809=CARTESIAN_POINT('Ctrl Pts',(7.12820716890676,36.5396877093727,7.99265394943905));
#25810=CARTESIAN_POINT('Ctrl Pts',(7.10080210402623,36.5670927742533,7.9967480843909));
#25811=CARTESIAN_POINT('Ctrl Pts',(7.07724019794044,36.5832420563329,7.99969589327637));
#25812=CARTESIAN_POINT('Ctrl Pts',(7.02552293481357,36.6046977939649,8.00385029472357));
#25813=CARTESIAN_POINT('Ctrl Pts',(6.99736126101101,36.61,8.005));
#25814=CARTESIAN_POINT('Ctrl Pts',(6.9444587993513,36.61,8.005));
#25815=CARTESIAN_POINT('Ctrl Pts',(6.91629712554875,36.6046977939649,8.00385029472357));
#25816=CARTESIAN_POINT('Ctrl Pts',(6.86457986242187,36.5832420563329,7.99969589327637));
#25817=CARTESIAN_POINT('Ctrl Pts',(6.84101795633608,36.5670927742533,7.9967480843909));
#25818=CARTESIAN_POINT('Ctrl Pts',(6.81361289145555,36.5396877093727,7.99265394943905));
#25819=CARTESIAN_POINT('Ctrl Pts',(6.80531516486984,36.5298014223953,7.99129192197638));
#25820=CARTESIAN_POINT('Ctrl Pts',(6.7979215912611,36.5190588089979,7.99));
#25821=CARTESIAN_POINT('Origin',(6.97091003018116,36.4,7.99));
#25822=CARTESIAN_POINT('',(6.7979215912611,35.8,7.99));
#25823=CARTESIAN_POINT('Origin',(6.97091003018116,35.8,7.));
#25824=CARTESIAN_POINT('',(5.96591003018116,37.,7.));
#25825=CARTESIAN_POINT('Origin',(6.97091003018116,37.,7.));
#25826=CARTESIAN_POINT('',(5.96591003018116,35.8,7.));
#25827=CARTESIAN_POINT('',(5.96591003018116,35.8,7.));
#25828=CARTESIAN_POINT('Origin',(6.97091003018116,35.8,7.));
#25829=CARTESIAN_POINT('Origin',(6.97091003018116,35.8,7.));
#25830=CARTESIAN_POINT('',(5.17091003018116,37.,7.));
#25831=CARTESIAN_POINT('Origin',(6.97091003018116,37.,7.));
#25832=CARTESIAN_POINT('',(5.17091003018116,35.8,7.));
#25833=CARTESIAN_POINT('',(5.17091003018116,35.8,7.));
#25834=CARTESIAN_POINT('Origin',(6.97091003018116,35.8,7.));
#25835=CARTESIAN_POINT('Origin',(6.97091003018116,37.,7.));
#25836=CARTESIAN_POINT('Origin',(6.97091003018116,35.8,7.));
#25837=CARTESIAN_POINT('',(0.,0.,0.));
#25838=CARTESIAN_POINT('Origin',(0.,-0.5,0.));
#25839=CARTESIAN_POINT('',(-1.,-0.375,-6.12323399573677E-17));
#25840=CARTESIAN_POINT('',(-0.992156741649222,-0.5,0.125));
#25841=CARTESIAN_POINT('Ctrl Pts',(-1.,-0.375,-1.00613961606655E-16));
#25842=CARTESIAN_POINT('Ctrl Pts',(-1.,-0.375,0.0157128711428661));
#25843=CARTESIAN_POINT('Ctrl Pts',(-0.999591823858855,-0.378143583103513,
0.0324619190698278));
#25844=CARTESIAN_POINT('Ctrl Pts',(-0.998116453123232,-0.390905426591754,
0.0632545375991437));
#25845=CARTESIAN_POINT('Ctrl Pts',(-0.997070068816062,-0.400522781657727,
0.0772994769543643));
#25846=CARTESIAN_POINT('Ctrl Pts',(-0.995102104277285,-0.422700615683787,
0.0994773109804239));
#25847=CARTESIAN_POINT('Ctrl Pts',(-0.994052129228928,-0.436745514765346,
0.109094593469654));
#25848=CARTESIAN_POINT('Ctrl Pts',(-0.99256853061881,-0.467537996927464,
0.121856383722779));
#25849=CARTESIAN_POINT('Ctrl Pts',(-0.992156741649222,-0.484286997589363,
0.125));
#25850=CARTESIAN_POINT('Ctrl Pts',(-0.992156741649222,-0.5,0.125));
#25851=CARTESIAN_POINT('',(-1.,-0.625,-6.12323399573677E-17));
#25852=CARTESIAN_POINT('Ctrl Pts',(-1.,-0.625,-4.5102810375397E-17));
#25853=CARTESIAN_POINT('Ctrl Pts',(-1.,-0.625,-0.0157128711428662));
#25854=CARTESIAN_POINT('Ctrl Pts',(-0.999591823858855,-0.621856416896487,
-0.032461919069828));
#25855=CARTESIAN_POINT('Ctrl Pts',(-0.998116453123232,-0.609094573408246,
-0.0632545375991439));
#25856=CARTESIAN_POINT('Ctrl Pts',(-0.997070068816062,-0.599477218342273,
-0.0772994769543645));
#25857=CARTESIAN_POINT('Ctrl Pts',(-0.995102104277285,-0.577299384316213,
-0.0994773109804241));
#25858=CARTESIAN_POINT('Ctrl Pts',(-0.994052129228928,-0.563254485234654,
-0.109094593469655));
#25859=CARTESIAN_POINT('Ctrl Pts',(-0.99256853061881,-0.532462003072536,
-0.121856383722779));
#25860=CARTESIAN_POINT('Ctrl Pts',(-0.992156741649221,-0.515713002410637,
-0.125));
#25861=CARTESIAN_POINT('Ctrl Pts',(-0.992156741649221,-0.484286997589363,
-0.125));
#25862=CARTESIAN_POINT('Ctrl Pts',(-0.99256853061881,-0.467537996927464,
-0.121856383722779));
#25863=CARTESIAN_POINT('Ctrl Pts',(-0.994052129228928,-0.436745514765346,
-0.109094593469655));
#25864=CARTESIAN_POINT('Ctrl Pts',(-0.995102104277285,-0.422700615683787,
-0.0994773109804241));
#25865=CARTESIAN_POINT('Ctrl Pts',(-0.997070068816062,-0.400522781657728,
-0.0772994769543645));
#25866=CARTESIAN_POINT('Ctrl Pts',(-0.998116453123232,-0.390905426591754,
-0.063254537599144));
#25867=CARTESIAN_POINT('Ctrl Pts',(-0.999591823858855,-0.378143583103513,
-0.0324619190698281));
#25868=CARTESIAN_POINT('Ctrl Pts',(-1.,-0.375,-0.0157128711428663));
#25869=CARTESIAN_POINT('Ctrl Pts',(-1.,-0.375,-9.36750677027476E-17));
#25870=CARTESIAN_POINT('Ctrl Pts',(-0.992156741649222,-0.5,0.125));
#25871=CARTESIAN_POINT('Ctrl Pts',(-0.992156741649222,-0.515713002410637,
0.125));
#25872=CARTESIAN_POINT('Ctrl Pts',(-0.99256853061881,-0.532462003072536,
0.121856383722779));
#25873=CARTESIAN_POINT('Ctrl Pts',(-0.994052129228928,-0.563254485234654,
0.109094593469654));
#25874=CARTESIAN_POINT('Ctrl Pts',(-0.995102104277285,-0.577299384316213,
0.0994773109804241));
#25875=CARTESIAN_POINT('Ctrl Pts',(-0.997070068816062,-0.599477218342273,
0.0772994769543644));
#25876=CARTESIAN_POINT('Ctrl Pts',(-0.998116453123232,-0.609094573408246,
0.0632545375991438));
#25877=CARTESIAN_POINT('Ctrl Pts',(-0.999591823858855,-0.621856416896487,
0.0324619190698279));
#25878=CARTESIAN_POINT('Ctrl Pts',(-1.,-0.625,0.0157128711428661));
#25879=CARTESIAN_POINT('Ctrl Pts',(-1.,-0.625,-4.85722573273506E-17));
#25880=CARTESIAN_POINT('',(-0.586834729715275,-0.5,0.125));
#25881=CARTESIAN_POINT('',(-7.65404249467096E-18,-0.5,0.125));
#25882=CARTESIAN_POINT('',(-0.6,-0.625,1.24532753107453E-17));
#25883=CARTESIAN_POINT('Ctrl Pts',(-0.6,-0.625,-4.16333634234434E-17));
#25884=CARTESIAN_POINT('Ctrl Pts',(-0.6,-0.625,0.0157444828659572));
#25885=CARTESIAN_POINT('Ctrl Pts',(-0.599317707212167,-0.621844041497889,
0.0325072544867633));
#25886=CARTESIAN_POINT('Ctrl Pts',(-0.596852269967858,-0.609072857638709,
0.0632914182239686));
#25887=CARTESIAN_POINT('Ctrl Pts',(-0.59510289473619,-0.599460146728784,
0.077316548567853));
#25888=CARTESIAN_POINT('Ctrl Pts',(-0.591804743154611,-0.577315815675743,
0.0994608796208941));
#25889=CARTESIAN_POINT('Ctrl Pts',(-0.590038488226116,-0.563290995658393,
0.109073016834181));
#25890=CARTESIAN_POINT('Ctrl Pts',(-0.587534197873268,-0.532507913768158,
0.121843784097853));
#25891=CARTESIAN_POINT('Ctrl Pts',(-0.586834729715275,-0.515745525063995,
0.125));
#25892=CARTESIAN_POINT('Ctrl Pts',(-0.586834729715275,-0.5,0.125));
#25893=CARTESIAN_POINT('',(-0.586834729715275,-0.5,-0.125));
#25894=CARTESIAN_POINT('Ctrl Pts',(-0.586834729715275,-0.5,-0.125));
#25895=CARTESIAN_POINT('Ctrl Pts',(-0.586834729715275,-0.515745525063995,
-0.125));
#25896=CARTESIAN_POINT('Ctrl Pts',(-0.587534197873268,-0.532507913768158,
-0.121843784097853));
#25897=CARTESIAN_POINT('Ctrl Pts',(-0.590038488226116,-0.563290995658393,
-0.109073016834181));
#25898=CARTESIAN_POINT('Ctrl Pts',(-0.591804743154611,-0.577315815675743,
-0.0994608796208942));
#25899=CARTESIAN_POINT('Ctrl Pts',(-0.59510289473619,-0.599460146728784,
-0.0773165485678531));
#25900=CARTESIAN_POINT('Ctrl Pts',(-0.596852269967858,-0.609072857638709,
-0.0632914182239687));
#25901=CARTESIAN_POINT('Ctrl Pts',(-0.599317707212167,-0.621844041497889,
-0.0325072544867635));
#25902=CARTESIAN_POINT('Ctrl Pts',(-0.6,-0.625,-0.0157444828659573));
#25903=CARTESIAN_POINT('Ctrl Pts',(-0.6,-0.625,-5.20417042793042E-17));
#25904=CARTESIAN_POINT('',(-0.6,-0.375,3.50046804984438E-17));
#25905=CARTESIAN_POINT('Ctrl Pts',(-0.6,-0.375,-3.46944695195361E-18));
#25906=CARTESIAN_POINT('Ctrl Pts',(-0.6,-0.375,-0.0157444828659572));
#25907=CARTESIAN_POINT('Ctrl Pts',(-0.599317707212167,-0.378155958502111,
-0.0325072544867634));
#25908=CARTESIAN_POINT('Ctrl Pts',(-0.596852269967858,-0.390927142361291,
-0.0632914182239686));
#25909=CARTESIAN_POINT('Ctrl Pts',(-0.59510289473619,-0.400539853271216,
-0.077316548567853));
#25910=CARTESIAN_POINT('Ctrl Pts',(-0.591804743154611,-0.422684184324257,
-0.0994608796208942));
#25911=CARTESIAN_POINT('Ctrl Pts',(-0.590038488226116,-0.436709004341607,
-0.109073016834181));
#25912=CARTESIAN_POINT('Ctrl Pts',(-0.587534197873268,-0.467492086231842,
-0.121843784097853));
#25913=CARTESIAN_POINT('Ctrl Pts',(-0.586834729715275,-0.484254474936005,
-0.125));
#25914=CARTESIAN_POINT('Ctrl Pts',(-0.586834729715275,-0.5,-0.125));
#25915=CARTESIAN_POINT('Ctrl Pts',(-0.586834729715275,-0.5,0.125));
#25916=CARTESIAN_POINT('Ctrl Pts',(-0.586834729715275,-0.484254474936005,
0.125));
#25917=CARTESIAN_POINT('Ctrl Pts',(-0.587534197873268,-0.467492086231842,
0.121843784097853));
#25918=CARTESIAN_POINT('Ctrl Pts',(-0.590038488226116,-0.436709004341607,
0.109073016834181));
#25919=CARTESIAN_POINT('Ctrl Pts',(-0.591804743154611,-0.422684184324257,
0.0994608796208941));
#25920=CARTESIAN_POINT('Ctrl Pts',(-0.59510289473619,-0.400539853271216,
0.077316548567853));
#25921=CARTESIAN_POINT('Ctrl Pts',(-0.596852269967858,-0.390927142361291,
0.0632914182239686));
#25922=CARTESIAN_POINT('Ctrl Pts',(-0.599317707212167,-0.378155958502111,
0.0325072544867634));
#25923=CARTESIAN_POINT('Ctrl Pts',(-0.6,-0.375,0.0157444828659572));
#25924=CARTESIAN_POINT('Ctrl Pts',(-0.6,-0.375,-2.42861286636753E-17));
#25925=CARTESIAN_POINT('Origin',(0.,-0.5,0.));
#25926=CARTESIAN_POINT('',(0.586834729715275,-0.5,-0.125));
#25927=CARTESIAN_POINT('',(0.586834729715275,-0.5,0.125));
#25928=CARTESIAN_POINT('Ctrl Pts',(0.586834729715275,-0.5,-0.125));
#25929=CARTESIAN_POINT('Ctrl Pts',(0.586834729715275,-0.484254474936005,
-0.125));
#25930=CARTESIAN_POINT('Ctrl Pts',(0.587534197873268,-0.467492086231842,
-0.121843784097853));
#25931=CARTESIAN_POINT('Ctrl Pts',(0.590038488226116,-0.436709004341607,
-0.109073016834181));
#25932=CARTESIAN_POINT('Ctrl Pts',(0.591804743154611,-0.422684184324257,
-0.0994608796208941));
#25933=CARTESIAN_POINT('Ctrl Pts',(0.59510289473619,-0.400539853271216,
-0.0773165485678529));
#25934=CARTESIAN_POINT('Ctrl Pts',(0.596852269967858,-0.390927142361291,
-0.0632914182239686));
#25935=CARTESIAN_POINT('Ctrl Pts',(0.599317707212167,-0.378155958502111,
-0.0325072544867633));
#25936=CARTESIAN_POINT('Ctrl Pts',(0.6,-0.375,-0.0157444828659572));
#25937=CARTESIAN_POINT('Ctrl Pts',(0.6,-0.375,0.0157444828659573));
#25938=CARTESIAN_POINT('Ctrl Pts',(0.599317707212167,-0.378155958502111,
0.0325072544867635));
#25939=CARTESIAN_POINT('Ctrl Pts',(0.596852269967858,-0.390927142361291,
0.0632914182239687));
#25940=CARTESIAN_POINT('Ctrl Pts',(0.59510289473619,-0.400539853271216,
0.0773165485678531));
#25941=CARTESIAN_POINT('Ctrl Pts',(0.591804743154611,-0.422684184324257,
0.0994608796208942));
#25942=CARTESIAN_POINT('Ctrl Pts',(0.590038488226116,-0.436709004341607,
0.109073016834181));
#25943=CARTESIAN_POINT('Ctrl Pts',(0.587534197873268,-0.467492086231842,
0.121843784097853));
#25944=CARTESIAN_POINT('Ctrl Pts',(0.586834729715275,-0.484254474936005,
0.125));
#25945=CARTESIAN_POINT('Ctrl Pts',(0.586834729715275,-0.5,0.125));
#25946=CARTESIAN_POINT('Ctrl Pts',(0.586834729715275,-0.5,0.125));
#25947=CARTESIAN_POINT('Ctrl Pts',(0.586834729715275,-0.515745525063995,
0.125));
#25948=CARTESIAN_POINT('Ctrl Pts',(0.587534197873268,-0.532507913768158,
0.121843784097853));
#25949=CARTESIAN_POINT('Ctrl Pts',(0.590038488226116,-0.563290995658393,
0.109073016834181));
#25950=CARTESIAN_POINT('Ctrl Pts',(0.591804743154611,-0.577315815675743,
0.0994608796208942));
#25951=CARTESIAN_POINT('Ctrl Pts',(0.59510289473619,-0.599460146728784,
0.077316548567853));
#25952=CARTESIAN_POINT('Ctrl Pts',(0.596852269967858,-0.609072857638709,
0.0632914182239688));
#25953=CARTESIAN_POINT('Ctrl Pts',(0.599317707212167,-0.621844041497889,
0.0325072544867635));
#25954=CARTESIAN_POINT('Ctrl Pts',(0.6,-0.625,0.0157444828659573));
#25955=CARTESIAN_POINT('Ctrl Pts',(0.6,-0.625,-0.0157444828659572));
#25956=CARTESIAN_POINT('Ctrl Pts',(0.599317707212167,-0.621844041497889,
-0.0325072544867633));
#25957=CARTESIAN_POINT('Ctrl Pts',(0.596852269967858,-0.609072857638709,
-0.0632914182239685));
#25958=CARTESIAN_POINT('Ctrl Pts',(0.59510289473619,-0.599460146728784,
-0.077316548567853));
#25959=CARTESIAN_POINT('Ctrl Pts',(0.591804743154611,-0.577315815675743,
-0.0994608796208941));
#25960=CARTESIAN_POINT('Ctrl Pts',(0.590038488226116,-0.563290995658393,
-0.10907301683418));
#25961=CARTESIAN_POINT('Ctrl Pts',(0.587534197873268,-0.532507913768158,
-0.121843784097853));
#25962=CARTESIAN_POINT('Ctrl Pts',(0.586834729715275,-0.515745525063995,
-0.125));
#25963=CARTESIAN_POINT('Ctrl Pts',(0.586834729715275,-0.5,-0.125));
#25964=CARTESIAN_POINT('',(0.992156741649222,-0.5,0.125));
#25965=CARTESIAN_POINT('',(-7.65404249467096E-18,-0.5,0.125));
#25966=CARTESIAN_POINT('',(1.,-0.625,6.12323399573677E-17));
#25967=CARTESIAN_POINT('Ctrl Pts',(1.,-0.625,7.28583859910259E-17));
#25968=CARTESIAN_POINT('Ctrl Pts',(1.,-0.625,0.0157128711428663));
#25969=CARTESIAN_POINT('Ctrl Pts',(0.999591823858855,-0.621856416896487,
0.032461919069828));
#25970=CARTESIAN_POINT('Ctrl Pts',(0.998116453123232,-0.609094573408246,
0.0632545375991439));
#25971=CARTESIAN_POINT('Ctrl Pts',(0.997070068816062,-0.599477218342273,
0.0772994769543645));
#25972=CARTESIAN_POINT('Ctrl Pts',(0.995102104277285,-0.577299384316213,
0.0994773109804242));
#25973=CARTESIAN_POINT('Ctrl Pts',(0.994052129228928,-0.563254485234654,
0.109094593469655));
#25974=CARTESIAN_POINT('Ctrl Pts',(0.99256853061881,-0.532462003072536,
0.121856383722779));
#25975=CARTESIAN_POINT('Ctrl Pts',(0.992156741649222,-0.515713002410637,
0.125));
#25976=CARTESIAN_POINT('Ctrl Pts',(0.992156741649222,-0.5,0.125));
#25977=CARTESIAN_POINT('',(1.,-0.375,6.12323399573677E-17));
#25978=CARTESIAN_POINT('Ctrl Pts',(1.,-0.375,2.08166817117217E-17));
#25979=CARTESIAN_POINT('Ctrl Pts',(1.,-0.375,-0.0157128711428662));
#25980=CARTESIAN_POINT('Ctrl Pts',(0.999591823858855,-0.378143583103513,
-0.032461919069828));
#25981=CARTESIAN_POINT('Ctrl Pts',(0.998116453123232,-0.390905426591754,
-0.0632545375991438));
#25982=CARTESIAN_POINT('Ctrl Pts',(0.997070068816062,-0.400522781657728,
-0.0772994769543644));
#25983=CARTESIAN_POINT('Ctrl Pts',(0.995102104277285,-0.422700615683787,
-0.099477310980424));
#25984=CARTESIAN_POINT('Ctrl Pts',(0.994052129228928,-0.436745514765346,
-0.109094593469654));
#25985=CARTESIAN_POINT('Ctrl Pts',(0.99256853061881,-0.467537996927464,
-0.121856383722779));
#25986=CARTESIAN_POINT('Ctrl Pts',(0.992156741649222,-0.484286997589363,
-0.125));
#25987=CARTESIAN_POINT('Ctrl Pts',(0.992156741649222,-0.515713002410637,
-0.125));
#25988=CARTESIAN_POINT('Ctrl Pts',(0.99256853061881,-0.532462003072536,
-0.121856383722779));
#25989=CARTESIAN_POINT('Ctrl Pts',(0.994052129228928,-0.563254485234654,
-0.109094593469654));
#25990=CARTESIAN_POINT('Ctrl Pts',(0.995102104277285,-0.577299384316213,
-0.099477310980424));
#25991=CARTESIAN_POINT('Ctrl Pts',(0.997070068816062,-0.599477218342273,
-0.0772994769543643));
#25992=CARTESIAN_POINT('Ctrl Pts',(0.998116453123232,-0.609094573408246,
-0.0632545375991438));
#25993=CARTESIAN_POINT('Ctrl Pts',(0.999591823858855,-0.621856416896487,
-0.0324619190698279));
#25994=CARTESIAN_POINT('Ctrl Pts',(1.,-0.625,-0.0157128711428661));
#25995=CARTESIAN_POINT('Ctrl Pts',(1.,-0.625,8.32667268468867E-17));
#25996=CARTESIAN_POINT('Ctrl Pts',(0.992156741649222,-0.5,0.125));
#25997=CARTESIAN_POINT('Ctrl Pts',(0.992156741649222,-0.484286997589363,
0.125));
#25998=CARTESIAN_POINT('Ctrl Pts',(0.99256853061881,-0.467537996927464,
0.121856383722779));
#25999=CARTESIAN_POINT('Ctrl Pts',(0.994052129228928,-0.436745514765346,
0.109094593469654));
#26000=CARTESIAN_POINT('Ctrl Pts',(0.995102104277285,-0.422700615683787,
0.0994773109804241));
#26001=CARTESIAN_POINT('Ctrl Pts',(0.997070068816062,-0.400522781657727,
0.0772994769543644));
#26002=CARTESIAN_POINT('Ctrl Pts',(0.998116453123232,-0.390905426591754,
0.0632545375991438));
#26003=CARTESIAN_POINT('Ctrl Pts',(0.999591823858855,-0.378143583103513,
0.0324619190698279));
#26004=CARTESIAN_POINT('Ctrl Pts',(1.,-0.375,0.0157128711428662));
#26005=CARTESIAN_POINT('Ctrl Pts',(1.,-0.375,2.77555756156289E-17));
#26006=CARTESIAN_POINT('Origin',(0.,-0.1,0.));
#26007=CARTESIAN_POINT('',(-1.,-0.9,1.22464679914735E-16));
#26008=CARTESIAN_POINT('Origin',(0.,-0.9,0.));
#26009=CARTESIAN_POINT('',(-1.,-0.1,-1.22464679914735E-16));
#26010=CARTESIAN_POINT('',(-1.,-0.1,1.22464679914735E-16));
#26011=CARTESIAN_POINT('',(-1.,-0.1,-1.22464679914735E-16));
#26012=CARTESIAN_POINT('Origin',(0.,-0.1,0.));
#26013=CARTESIAN_POINT('',(0.,-0.625,-1.));
#26014=CARTESIAN_POINT('',(0.,-0.375,-1.));
#26015=CARTESIAN_POINT('Ctrl Pts',(-2.08166817117217E-17,-0.625,-1.));
#26016=CARTESIAN_POINT('Ctrl Pts',(0.0157128711428662,-0.625,-1.));
#26017=CARTESIAN_POINT('Ctrl Pts',(0.0324619190698279,-0.621856416896487,
-0.999591823858855));
#26018=CARTESIAN_POINT('Ctrl Pts',(0.0632545375991438,-0.609094573408246,
-0.998116453123232));
#26019=CARTESIAN_POINT('Ctrl Pts',(0.0772994769543644,-0.599477218342273,
-0.997070068816062));
#26020=CARTESIAN_POINT('Ctrl Pts',(0.0994773109804241,-0.577299384316213,
-0.995102104277285));
#26021=CARTESIAN_POINT('Ctrl Pts',(0.109094593469654,-0.563254485234654,
-0.994052129228928));
#26022=CARTESIAN_POINT('Ctrl Pts',(0.121856383722779,-0.532462003072536,
-0.99256853061881));
#26023=CARTESIAN_POINT('Ctrl Pts',(0.125,-0.515713002410637,-0.992156741649221));
#26024=CARTESIAN_POINT('Ctrl Pts',(0.125,-0.484286997589363,-0.992156741649221));
#26025=CARTESIAN_POINT('Ctrl Pts',(0.121856383722779,-0.467537996927464,
-0.99256853061881));
#26026=CARTESIAN_POINT('Ctrl Pts',(0.109094593469654,-0.436745514765346,
-0.994052129228928));
#26027=CARTESIAN_POINT('Ctrl Pts',(0.0994773109804241,-0.422700615683787,
-0.995102104277285));
#26028=CARTESIAN_POINT('Ctrl Pts',(0.0772994769543645,-0.400522781657728,
-0.997070068816062));
#26029=CARTESIAN_POINT('Ctrl Pts',(0.0632545375991439,-0.390905426591754,
-0.998116453123232));
#26030=CARTESIAN_POINT('Ctrl Pts',(0.032461919069828,-0.378143583103513,
-0.999591823858855));
#26031=CARTESIAN_POINT('Ctrl Pts',(0.0157128711428662,-0.375,-1.));
#26032=CARTESIAN_POINT('Ctrl Pts',(3.81639164714898E-17,-0.375,-1.));
#26033=CARTESIAN_POINT('',(-0.125,-0.5,-0.992156741649222));
#26034=CARTESIAN_POINT('Ctrl Pts',(4.5102810375397E-17,-0.375,-1.));
#26035=CARTESIAN_POINT('Ctrl Pts',(-0.0157128711428661,-0.375,-1.));
#26036=CARTESIAN_POINT('Ctrl Pts',(-0.0324619190698279,-0.378143583103513,
-0.999591823858855));
#26037=CARTESIAN_POINT('Ctrl Pts',(-0.0632545375991437,-0.390905426591754,
-0.998116453123232));
#26038=CARTESIAN_POINT('Ctrl Pts',(-0.0772994769543643,-0.400522781657727,
-0.997070068816062));
#26039=CARTESIAN_POINT('Ctrl Pts',(-0.099477310980424,-0.422700615683787,
-0.995102104277285));
#26040=CARTESIAN_POINT('Ctrl Pts',(-0.109094593469654,-0.436745514765346,
-0.994052129228928));
#26041=CARTESIAN_POINT('Ctrl Pts',(-0.121856383722779,-0.467537996927464,
-0.99256853061881));
#26042=CARTESIAN_POINT('Ctrl Pts',(-0.125,-0.484286997589363,-0.992156741649222));
#26043=CARTESIAN_POINT('Ctrl Pts',(-0.125,-0.5,-0.992156741649222));
#26044=CARTESIAN_POINT('Ctrl Pts',(-0.125,-0.5,-0.992156741649222));
#26045=CARTESIAN_POINT('Ctrl Pts',(-0.125,-0.515713002410637,-0.992156741649222));
#26046=CARTESIAN_POINT('Ctrl Pts',(-0.121856383722779,-0.532462003072536,
-0.99256853061881));
#26047=CARTESIAN_POINT('Ctrl Pts',(-0.109094593469654,-0.563254485234654,
-0.994052129228928));
#26048=CARTESIAN_POINT('Ctrl Pts',(-0.0994773109804241,-0.577299384316213,
-0.995102104277285));
#26049=CARTESIAN_POINT('Ctrl Pts',(-0.0772994769543644,-0.599477218342273,
-0.997070068816062));
#26050=CARTESIAN_POINT('Ctrl Pts',(-0.0632545375991439,-0.609094573408246,
-0.998116453123232));
#26051=CARTESIAN_POINT('Ctrl Pts',(-0.032461919069828,-0.621856416896487,
-0.999591823858855));
#26052=CARTESIAN_POINT('Ctrl Pts',(-0.0157128711428662,-0.625,-1.));
#26053=CARTESIAN_POINT('Ctrl Pts',(-1.38777878078145E-17,-0.625,-1.));
#26054=CARTESIAN_POINT('',(0.,-0.375,1.));
#26055=CARTESIAN_POINT('',(0.,-0.625,1.));
#26056=CARTESIAN_POINT('Ctrl Pts',(4.16333634234434E-17,-0.375,1.));
#26057=CARTESIAN_POINT('Ctrl Pts',(0.0157128711428662,-0.375,1.));
#26058=CARTESIAN_POINT('Ctrl Pts',(0.032461919069828,-0.378143583103513,
0.999591823858855));
#26059=CARTESIAN_POINT('Ctrl Pts',(0.0632545375991439,-0.390905426591754,
0.998116453123232));
#26060=CARTESIAN_POINT('Ctrl Pts',(0.0772994769543644,-0.400522781657728,
0.997070068816062));
#26061=CARTESIAN_POINT('Ctrl Pts',(0.0994773109804241,-0.422700615683787,
0.995102104277285));
#26062=CARTESIAN_POINT('Ctrl Pts',(0.109094593469654,-0.436745514765346,
0.994052129228928));
#26063=CARTESIAN_POINT('Ctrl Pts',(0.121856383722779,-0.467537996927464,
0.99256853061881));
#26064=CARTESIAN_POINT('Ctrl Pts',(0.125,-0.484286997589363,0.992156741649222));
#26065=CARTESIAN_POINT('Ctrl Pts',(0.125,-0.515713002410637,0.992156741649222));
#26066=CARTESIAN_POINT('Ctrl Pts',(0.121856383722779,-0.532462003072536,
0.99256853061881));
#26067=CARTESIAN_POINT('Ctrl Pts',(0.109094593469655,-0.563254485234654,
0.994052129228928));
#26068=CARTESIAN_POINT('Ctrl Pts',(0.0994773109804241,-0.577299384316213,
0.995102104277285));
#26069=CARTESIAN_POINT('Ctrl Pts',(0.0772994769543644,-0.599477218342273,
0.997070068816062));
#26070=CARTESIAN_POINT('Ctrl Pts',(0.0632545375991438,-0.609094573408246,
0.998116453123232));
#26071=CARTESIAN_POINT('Ctrl Pts',(0.0324619190698279,-0.621856416896487,
0.999591823858855));
#26072=CARTESIAN_POINT('Ctrl Pts',(0.0157128711428662,-0.625,1.));
#26073=CARTESIAN_POINT('Ctrl Pts',(-1.73472347597681E-17,-0.625,1.));
#26074=CARTESIAN_POINT('',(-0.125,-0.5,0.992156741649222));
#26075=CARTESIAN_POINT('Ctrl Pts',(-1.73472347597681E-17,-0.625,1.));
#26076=CARTESIAN_POINT('Ctrl Pts',(-0.0157128711428662,-0.625,1.));
#26077=CARTESIAN_POINT('Ctrl Pts',(-0.032461919069828,-0.621856416896487,
0.999591823858855));
#26078=CARTESIAN_POINT('Ctrl Pts',(-0.0632545375991439,-0.609094573408246,
0.998116453123232));
#26079=CARTESIAN_POINT('Ctrl Pts',(-0.0772994769543645,-0.599477218342273,
0.997070068816062));
#26080=CARTESIAN_POINT('Ctrl Pts',(-0.0994773109804241,-0.577299384316213,
0.995102104277285));
#26081=CARTESIAN_POINT('Ctrl Pts',(-0.109094593469654,-0.563254485234654,
0.994052129228928));
#26082=CARTESIAN_POINT('Ctrl Pts',(-0.121856383722779,-0.532462003072536,
0.99256853061881));
#26083=CARTESIAN_POINT('Ctrl Pts',(-0.125,-0.515713002410637,0.992156741649222));
#26084=CARTESIAN_POINT('Ctrl Pts',(-0.125,-0.5,0.992156741649222));
#26085=CARTESIAN_POINT('Ctrl Pts',(-0.125,-0.5,0.992156741649222));
#26086=CARTESIAN_POINT('Ctrl Pts',(-0.125,-0.484286997589363,0.992156741649222));
#26087=CARTESIAN_POINT('Ctrl Pts',(-0.121856383722779,-0.467537996927464,
0.99256853061881));
#26088=CARTESIAN_POINT('Ctrl Pts',(-0.109094593469654,-0.436745514765346,
0.994052129228928));
#26089=CARTESIAN_POINT('Ctrl Pts',(-0.099477310980424,-0.422700615683787,
0.995102104277285));
#26090=CARTESIAN_POINT('Ctrl Pts',(-0.0772994769543643,-0.400522781657727,
0.997070068816062));
#26091=CARTESIAN_POINT('Ctrl Pts',(-0.0632545375991438,-0.390905426591754,
0.998116453123232));
#26092=CARTESIAN_POINT('Ctrl Pts',(-0.0324619190698279,-0.378143583103513,
0.999591823858855));
#26093=CARTESIAN_POINT('Ctrl Pts',(-0.0157128711428661,-0.375,1.));
#26094=CARTESIAN_POINT('Ctrl Pts',(4.5102810375397E-17,-0.375,1.));
#26095=CARTESIAN_POINT('Origin',(0.,-0.5,0.));
#26096=CARTESIAN_POINT('',(-0.125,-0.5,-0.586834729715275));
#26097=CARTESIAN_POINT('',(-0.125,-0.5,0.));
#26098=CARTESIAN_POINT('',(0.125,-0.5,-0.586834729715275));
#26099=CARTESIAN_POINT('Ctrl Pts',(0.125,-0.5,-0.586834729715275));
#26100=CARTESIAN_POINT('Ctrl Pts',(0.125,-0.515745525063995,-0.586834729715275));
#26101=CARTESIAN_POINT('Ctrl Pts',(0.121843784097853,-0.532507913768158,
-0.587534197873268));
#26102=CARTESIAN_POINT('Ctrl Pts',(0.109073016834181,-0.563290995658393,
-0.590038488226116));
#26103=CARTESIAN_POINT('Ctrl Pts',(0.0994608796208942,-0.577315815675743,
-0.591804743154611));
#26104=CARTESIAN_POINT('Ctrl Pts',(0.077316548567853,-0.599460146728784,
-0.59510289473619));
#26105=CARTESIAN_POINT('Ctrl Pts',(0.0632914182239686,-0.609072857638709,
-0.596852269967858));
#26106=CARTESIAN_POINT('Ctrl Pts',(0.0325072544867633,-0.621844041497889,
-0.599317707212167));
#26107=CARTESIAN_POINT('Ctrl Pts',(0.0157444828659573,-0.625,-0.6));
#26108=CARTESIAN_POINT('Ctrl Pts',(-0.0157444828659572,-0.625,-0.6));
#26109=CARTESIAN_POINT('Ctrl Pts',(-0.0325072544867633,-0.621844041497889,
-0.599317707212167));
#26110=CARTESIAN_POINT('Ctrl Pts',(-0.0632914182239686,-0.609072857638709,
-0.596852269967858));
#26111=CARTESIAN_POINT('Ctrl Pts',(-0.077316548567853,-0.599460146728784,
-0.59510289473619));
#26112=CARTESIAN_POINT('Ctrl Pts',(-0.0994608796208941,-0.577315815675743,
-0.591804743154611));
#26113=CARTESIAN_POINT('Ctrl Pts',(-0.109073016834181,-0.563290995658393,
-0.590038488226116));
#26114=CARTESIAN_POINT('Ctrl Pts',(-0.121843784097853,-0.532507913768158,
-0.587534197873268));
#26115=CARTESIAN_POINT('Ctrl Pts',(-0.125,-0.515745525063995,-0.586834729715275));
#26116=CARTESIAN_POINT('Ctrl Pts',(-0.125,-0.5,-0.586834729715275));
#26117=CARTESIAN_POINT('Ctrl Pts',(-0.125,-0.5,-0.586834729715275));
#26118=CARTESIAN_POINT('Ctrl Pts',(-0.125,-0.484254474936005,-0.586834729715275));
#26119=CARTESIAN_POINT('Ctrl Pts',(-0.121843784097853,-0.467492086231842,
-0.587534197873268));
#26120=CARTESIAN_POINT('Ctrl Pts',(-0.109073016834181,-0.436709004341607,
-0.590038488226116));
#26121=CARTESIAN_POINT('Ctrl Pts',(-0.0994608796208942,-0.422684184324257,
-0.591804743154611));
#26122=CARTESIAN_POINT('Ctrl Pts',(-0.077316548567853,-0.400539853271216,
-0.59510289473619));
#26123=CARTESIAN_POINT('Ctrl Pts',(-0.0632914182239687,-0.39092714236129,
-0.596852269967858));
#26124=CARTESIAN_POINT('Ctrl Pts',(-0.0325072544867634,-0.378155958502111,
-0.599317707212167));
#26125=CARTESIAN_POINT('Ctrl Pts',(-0.0157444828659573,-0.375,-0.6));
#26126=CARTESIAN_POINT('Ctrl Pts',(0.0157444828659572,-0.375,-0.6));
#26127=CARTESIAN_POINT('Ctrl Pts',(0.0325072544867634,-0.378155958502111,
-0.599317707212167));
#26128=CARTESIAN_POINT('Ctrl Pts',(0.0632914182239686,-0.390927142361291,
-0.596852269967858));
#26129=CARTESIAN_POINT('Ctrl Pts',(0.077316548567853,-0.400539853271216,
-0.59510289473619));
#26130=CARTESIAN_POINT('Ctrl Pts',(0.0994608796208941,-0.422684184324257,
-0.591804743154611));
#26131=CARTESIAN_POINT('Ctrl Pts',(0.109073016834181,-0.436709004341607,
-0.590038488226116));
#26132=CARTESIAN_POINT('Ctrl Pts',(0.121843784097853,-0.467492086231842,
-0.587534197873268));
#26133=CARTESIAN_POINT('Ctrl Pts',(0.125,-0.484254474936005,-0.586834729715275));
#26134=CARTESIAN_POINT('Ctrl Pts',(0.125,-0.5,-0.586834729715275));
#26135=CARTESIAN_POINT('Origin',(0.,-0.5,0.));
#26136=CARTESIAN_POINT('',(0.125,-0.5,0.586834729715275));
#26137=CARTESIAN_POINT('',(-0.125,-0.5,0.586834729715275));
#26138=CARTESIAN_POINT('Ctrl Pts',(0.125,-0.5,0.586834729715275));
#26139=CARTESIAN_POINT('Ctrl Pts',(0.125,-0.484254474936005,0.586834729715275));
#26140=CARTESIAN_POINT('Ctrl Pts',(0.121843784097853,-0.467492086231842,
0.587534197873268));
#26141=CARTESIAN_POINT('Ctrl Pts',(0.109073016834181,-0.436709004341607,
0.590038488226116));
#26142=CARTESIAN_POINT('Ctrl Pts',(0.0994608796208941,-0.422684184324257,
0.591804743154611));
#26143=CARTESIAN_POINT('Ctrl Pts',(0.077316548567853,-0.400539853271216,
0.59510289473619));
#26144=CARTESIAN_POINT('Ctrl Pts',(0.0632914182239686,-0.390927142361291,
0.596852269967858));
#26145=CARTESIAN_POINT('Ctrl Pts',(0.0325072544867634,-0.378155958502111,
0.599317707212167));
#26146=CARTESIAN_POINT('Ctrl Pts',(0.0157444828659572,-0.375,0.6));
#26147=CARTESIAN_POINT('Ctrl Pts',(-0.0157444828659573,-0.375,0.6));
#26148=CARTESIAN_POINT('Ctrl Pts',(-0.0325072544867634,-0.378155958502111,
0.599317707212167));
#26149=CARTESIAN_POINT('Ctrl Pts',(-0.0632914182239687,-0.390927142361291,
0.596852269967858));
#26150=CARTESIAN_POINT('Ctrl Pts',(-0.077316548567853,-0.400539853271216,
0.59510289473619));
#26151=CARTESIAN_POINT('Ctrl Pts',(-0.0994608796208942,-0.422684184324257,
0.591804743154611));
#26152=CARTESIAN_POINT('Ctrl Pts',(-0.109073016834181,-0.436709004341607,
0.590038488226116));
#26153=CARTESIAN_POINT('Ctrl Pts',(-0.121843784097853,-0.467492086231842,
0.587534197873268));
#26154=CARTESIAN_POINT('Ctrl Pts',(-0.125,-0.484254474936005,0.586834729715275));
#26155=CARTESIAN_POINT('Ctrl Pts',(-0.125,-0.5,0.586834729715275));
#26156=CARTESIAN_POINT('Ctrl Pts',(-0.125,-0.5,0.586834729715275));
#26157=CARTESIAN_POINT('Ctrl Pts',(-0.125,-0.515745525063995,0.586834729715275));
#26158=CARTESIAN_POINT('Ctrl Pts',(-0.121843784097853,-0.532507913768158,
0.587534197873268));
#26159=CARTESIAN_POINT('Ctrl Pts',(-0.109073016834181,-0.563290995658393,
0.590038488226116));
#26160=CARTESIAN_POINT('Ctrl Pts',(-0.0994608796208941,-0.577315815675743,
0.591804743154611));
#26161=CARTESIAN_POINT('Ctrl Pts',(-0.077316548567853,-0.599460146728784,
0.59510289473619));
#26162=CARTESIAN_POINT('Ctrl Pts',(-0.0632914182239687,-0.609072857638709,
0.596852269967858));
#26163=CARTESIAN_POINT('Ctrl Pts',(-0.0325072544867635,-0.621844041497889,
0.599317707212167));
#26164=CARTESIAN_POINT('Ctrl Pts',(-0.0157444828659572,-0.625,0.6));
#26165=CARTESIAN_POINT('Ctrl Pts',(0.0157444828659572,-0.625,0.6));
#26166=CARTESIAN_POINT('Ctrl Pts',(0.0325072544867633,-0.621844041497889,
0.599317707212167));
#26167=CARTESIAN_POINT('Ctrl Pts',(0.0632914182239686,-0.609072857638709,
0.596852269967858));
#26168=CARTESIAN_POINT('Ctrl Pts',(0.077316548567853,-0.599460146728784,
0.59510289473619));
#26169=CARTESIAN_POINT('Ctrl Pts',(0.0994608796208942,-0.577315815675743,
0.591804743154611));
#26170=CARTESIAN_POINT('Ctrl Pts',(0.109073016834181,-0.563290995658393,
0.590038488226116));
#26171=CARTESIAN_POINT('Ctrl Pts',(0.121843784097853,-0.532507913768158,
0.587534197873268));
#26172=CARTESIAN_POINT('Ctrl Pts',(0.125,-0.515745525063995,0.586834729715275));
#26173=CARTESIAN_POINT('Ctrl Pts',(0.125,-0.5,0.586834729715275));
#26174=CARTESIAN_POINT('',(-0.125,-0.5,0.));
#26175=CARTESIAN_POINT('Origin',(0.,0.,0.));
#26176=CARTESIAN_POINT('',(-0.6,-0.9,7.34788079488412E-17));
#26177=CARTESIAN_POINT('Origin',(0.,-0.9,0.));
#26178=CARTESIAN_POINT('',(-0.6,0.,7.34788079488412E-17));
#26179=CARTESIAN_POINT('',(-0.6,0.85,-7.34788079488412E-17));
#26180=CARTESIAN_POINT('',(-0.6,0.,7.34788079488412E-17));
#26181=CARTESIAN_POINT('Origin',(0.,0.85,0.));
#26182=CARTESIAN_POINT('Origin',(0.,-0.9,0.));
#26183=CARTESIAN_POINT('Origin',(0.,0.,0.));
#26184=CARTESIAN_POINT('',(-1.4,0.,1.71450551880629E-16));
#26185=CARTESIAN_POINT('Origin',(0.,0.,0.));
#26186=CARTESIAN_POINT('',(1.23958209161204,0.,0.143317017690053));
#26187=CARTESIAN_POINT('',(1.22320001975977,0.,0.246749348660852));
#26188=CARTESIAN_POINT('Origin',(1.21321664662686,0.,0.192154639568406));
#26189=CARTESIAN_POINT('',(1.20190105810224,0.,0.335465908756113));
#26190=CARTESIAN_POINT('Origin',(0.,0.,0.));
#26191=CARTESIAN_POINT('',(1.16954029537568,0.,0.435062095450087));
#26192=CARTESIAN_POINT('Origin',(1.1682203282434,0.,0.379577794185952));
#26193=CARTESIAN_POINT('',(1.13462523166105,0.,0.519354515801077));
#26194=CARTESIAN_POINT('Origin',(0.,0.,0.));
#26195=CARTESIAN_POINT('',(1.08708260743774,0.,0.612662169561029));
#26196=CARTESIAN_POINT('Origin',(1.0944585482776,0.,0.557654483764164));
#26197=CARTESIAN_POINT('',(1.0394111664111,0.,0.690454891028201));
#26198=CARTESIAN_POINT('Origin',(0.,0.,0.));
#26199=CARTESIAN_POINT('',(0.977857337884349,0.,0.775176467748211));
#26200=CARTESIAN_POINT('Origin',(0.993747566553533,0.,0.72199986920298));
#26201=CARTESIAN_POINT('',(0.918603348636233,0.,0.844553975349804));
#26202=CARTESIAN_POINT('Origin',(0.,0.,0.));
#26203=CARTESIAN_POINT('',(0.844553975349804,0.,0.918603348636233));
#26204=CARTESIAN_POINT('Origin',(0.86856722168183,0.,0.86856722168183));
#26205=CARTESIAN_POINT('',(0.775176467748211,0.,0.977857337884349));
#26206=CARTESIAN_POINT('Origin',(0.,0.,0.));
#26207=CARTESIAN_POINT('',(0.690454891028201,0.,1.0394111664111));
#26208=CARTESIAN_POINT('Origin',(0.721999869202979,0.,0.993747566553533));
#26209=CARTESIAN_POINT('',(0.612662169561028,0.,1.08708260743774));
#26210=CARTESIAN_POINT('Origin',(0.,0.,0.));
#26211=CARTESIAN_POINT('',(0.519354515801077,0.,1.13462523166105));
#26212=CARTESIAN_POINT('Origin',(0.557654483764164,0.,1.0944585482776));
#26213=CARTESIAN_POINT('',(0.435062095450087,0.,1.16954029537568));
#26214=CARTESIAN_POINT('Origin',(0.,0.,0.));
#26215=CARTESIAN_POINT('',(0.335465908756113,0.,1.20190105810224));
#26216=CARTESIAN_POINT('Origin',(0.379577794185951,0.,1.1682203282434));
#26217=CARTESIAN_POINT('',(0.246749348660851,0.,1.22320001975977));
#26218=CARTESIAN_POINT('Origin',(0.,0.,0.));
#26219=CARTESIAN_POINT('',(0.143317017690053,0.,1.23958209161204));
#26220=CARTESIAN_POINT('Origin',(0.192154639568406,0.,1.21321664662686));
#26221=CARTESIAN_POINT('',(0.0523608139934478,0.,1.24674050008925));
#26222=CARTESIAN_POINT('Origin',(0.,0.,0.));
#26223=CARTESIAN_POINT('',(-0.0523608139934483,0.,1.24674050008925));
#26224=CARTESIAN_POINT('Origin',(-2.25642313758905E-16,0.,1.22833954473516));
#26225=CARTESIAN_POINT('',(-0.143317017690053,0.,1.23958209161204));
#26226=CARTESIAN_POINT('Origin',(0.,0.,0.));
#26227=CARTESIAN_POINT('',(-0.246749348660852,0.,1.22320001975977));
#26228=CARTESIAN_POINT('Origin',(-0.192154639568406,0.,1.21321664662686));
#26229=CARTESIAN_POINT('',(-0.335465908756113,0.,1.20190105810224));
#26230=CARTESIAN_POINT('Origin',(0.,0.,0.));
#26231=CARTESIAN_POINT('',(-0.435062095450087,0.,1.16954029537568));
#26232=CARTESIAN_POINT('Origin',(-0.379577794185951,0.,1.1682203282434));
#26233=CARTESIAN_POINT('',(-0.519354515801077,0.,1.13462523166105));
#26234=CARTESIAN_POINT('Origin',(0.,0.,0.));
#26235=CARTESIAN_POINT('',(-0.612662169561029,0.,1.08708260743774));
#26236=CARTESIAN_POINT('Origin',(-0.557654483764164,0.,1.0944585482776));
#26237=CARTESIAN_POINT('',(-0.690454891028201,0.,1.0394111664111));
#26238=CARTESIAN_POINT('Origin',(0.,0.,0.));
#26239=CARTESIAN_POINT('',(-0.775176467748211,0.,0.977857337884349));
#26240=CARTESIAN_POINT('Origin',(-0.721999869202979,0.,0.993747566553533));
#26241=CARTESIAN_POINT('',(-0.844553975349804,0.,0.918603348636233));
#26242=CARTESIAN_POINT('Origin',(0.,0.,0.));
#26243=CARTESIAN_POINT('',(-0.918603348636233,0.,0.844553975349804));
#26244=CARTESIAN_POINT('Origin',(-0.86856722168183,0.,0.86856722168183));
#26245=CARTESIAN_POINT('',(-0.977857337884348,0.,0.775176467748211));
#26246=CARTESIAN_POINT('Origin',(0.,0.,0.));
#26247=CARTESIAN_POINT('',(-1.0394111664111,0.,0.690454891028201));
#26248=CARTESIAN_POINT('Origin',(-0.993747566553533,0.,0.721999869202979));
#26249=CARTESIAN_POINT('',(-1.08708260743774,0.,0.612662169561028));
#26250=CARTESIAN_POINT('Origin',(0.,0.,0.));
#26251=CARTESIAN_POINT('',(-1.13462523166105,0.,0.519354515801077));
#26252=CARTESIAN_POINT('Origin',(-1.0944585482776,0.,0.557654483764164));
#26253=CARTESIAN_POINT('',(-1.16954029537568,0.,0.435062095450087));
#26254=CARTESIAN_POINT('Origin',(0.,0.,0.));
#26255=CARTESIAN_POINT('',(-1.20190105810224,0.,0.335465908756113));
#26256=CARTESIAN_POINT('Origin',(-1.1682203282434,0.,0.379577794185951));
#26257=CARTESIAN_POINT('',(-1.22320001975977,0.,0.246749348660851));
#26258=CARTESIAN_POINT('Origin',(0.,0.,0.));
#26259=CARTESIAN_POINT('',(-1.23958209161204,0.,0.143317017690053));
#26260=CARTESIAN_POINT('Origin',(-1.21321664662686,0.,0.192154639568406));
#26261=CARTESIAN_POINT('',(-1.24674050008925,0.,0.0523608139934479));
#26262=CARTESIAN_POINT('Origin',(0.,0.,0.));
#26263=CARTESIAN_POINT('',(-1.24674050008925,0.,-0.0523608139934482));
#26264=CARTESIAN_POINT('Origin',(-1.22833954473516,0.,-1.50428209172603E-16));
#26265=CARTESIAN_POINT('',(-1.23958209161204,0.,-0.143317017690053));
#26266=CARTESIAN_POINT('Origin',(0.,0.,0.));
#26267=CARTESIAN_POINT('',(-1.22320001975977,0.,-0.246749348660852));
#26268=CARTESIAN_POINT('Origin',(-1.21321664662686,0.,-0.192154639568406));
#26269=CARTESIAN_POINT('',(-1.20190105810224,0.,-0.335465908756113));
#26270=CARTESIAN_POINT('Origin',(0.,0.,0.));
#26271=CARTESIAN_POINT('',(-1.16954029537568,0.,-0.435062095450087));
#26272=CARTESIAN_POINT('Origin',(-1.1682203282434,0.,-0.379577794185951));
#26273=CARTESIAN_POINT('',(-1.13462523166105,0.,-0.519354515801077));
#26274=CARTESIAN_POINT('Origin',(0.,0.,0.));
#26275=CARTESIAN_POINT('',(-1.08708260743774,0.,-0.612662169561029));
#26276=CARTESIAN_POINT('Origin',(-1.0944585482776,0.,-0.557654483764164));
#26277=CARTESIAN_POINT('',(-1.0394111664111,0.,-0.690454891028201));
#26278=CARTESIAN_POINT('Origin',(0.,0.,0.));
#26279=CARTESIAN_POINT('',(-0.977857337884349,0.,-0.775176467748211));
#26280=CARTESIAN_POINT('Origin',(-0.993747566553533,0.,-0.721999869202979));
#26281=CARTESIAN_POINT('',(-0.918603348636233,0.,-0.844553975349804));
#26282=CARTESIAN_POINT('Origin',(0.,0.,0.));
#26283=CARTESIAN_POINT('',(-0.844553975349804,0.,-0.918603348636233));
#26284=CARTESIAN_POINT('Origin',(-0.86856722168183,0.,-0.86856722168183));
#26285=CARTESIAN_POINT('',(-0.775176467748211,0.,-0.977857337884348));
#26286=CARTESIAN_POINT('Origin',(0.,0.,0.));
#26287=CARTESIAN_POINT('',(-0.690454891028201,0.,-1.0394111664111));
#26288=CARTESIAN_POINT('Origin',(-0.721999869202979,0.,-0.993747566553533));
#26289=CARTESIAN_POINT('',(-0.612662169561028,0.,-1.08708260743774));
#26290=CARTESIAN_POINT('Origin',(0.,0.,0.));
#26291=CARTESIAN_POINT('',(-0.519354515801077,0.,-1.13462523166105));
#26292=CARTESIAN_POINT('Origin',(-0.557654483764164,0.,-1.0944585482776));
#26293=CARTESIAN_POINT('',(-0.435062095450087,0.,-1.16954029537568));
#26294=CARTESIAN_POINT('Origin',(0.,0.,0.));
#26295=CARTESIAN_POINT('',(-0.335465908756113,0.,-1.20190105810224));
#26296=CARTESIAN_POINT('Origin',(-0.379577794185951,0.,-1.1682203282434));
#26297=CARTESIAN_POINT('',(-0.246749348660852,0.,-1.22320001975977));
#26298=CARTESIAN_POINT('Origin',(0.,0.,0.));
#26299=CARTESIAN_POINT('',(-0.143317017690053,0.,-1.23958209161204));
#26300=CARTESIAN_POINT('Origin',(-0.192154639568406,0.,-1.21321664662686));
#26301=CARTESIAN_POINT('',(-0.0523608139934479,0.,-1.24674050008925));
#26302=CARTESIAN_POINT('Origin',(0.,0.,0.));
#26303=CARTESIAN_POINT('',(0.0523608139934481,0.,-1.24674050008925));
#26304=CARTESIAN_POINT('Origin',(7.52141045863017E-17,0.,-1.22833954473516));
#26305=CARTESIAN_POINT('',(0.143317017690053,0.,-1.23958209161204));
#26306=CARTESIAN_POINT('Origin',(0.,0.,0.));
#26307=CARTESIAN_POINT('',(0.246749348660852,0.,-1.22320001975977));
#26308=CARTESIAN_POINT('Origin',(0.192154639568406,0.,-1.21321664662686));
#26309=CARTESIAN_POINT('',(0.335465908756113,0.,-1.20190105810224));
#26310=CARTESIAN_POINT('Origin',(0.,0.,0.));
#26311=CARTESIAN_POINT('',(0.435062095450087,0.,-1.16954029537568));
#26312=CARTESIAN_POINT('Origin',(0.379577794185951,0.,-1.1682203282434));
#26313=CARTESIAN_POINT('',(0.519354515801077,0.,-1.13462523166105));
#26314=CARTESIAN_POINT('Origin',(0.,0.,0.));
#26315=CARTESIAN_POINT('',(0.612662169561028,0.,-1.08708260743774));
#26316=CARTESIAN_POINT('Origin',(0.557654483764164,0.,-1.0944585482776));
#26317=CARTESIAN_POINT('',(0.690454891028201,0.,-1.0394111664111));
#26318=CARTESIAN_POINT('Origin',(0.,0.,0.));
#26319=CARTESIAN_POINT('',(0.775176467748211,0.,-0.977857337884349));
#26320=CARTESIAN_POINT('Origin',(0.721999869202979,0.,-0.993747566553533));
#26321=CARTESIAN_POINT('',(0.844553975349804,0.,-0.918603348636233));
#26322=CARTESIAN_POINT('Origin',(0.,0.,0.));
#26323=CARTESIAN_POINT('',(0.918603348636233,0.,-0.844553975349804));
#26324=CARTESIAN_POINT('Origin',(0.86856722168183,0.,-0.86856722168183));
#26325=CARTESIAN_POINT('',(0.977857337884349,0.,-0.775176467748211));
#26326=CARTESIAN_POINT('Origin',(0.,0.,0.));
#26327=CARTESIAN_POINT('',(1.0394111664111,0.,-0.690454891028201));
#26328=CARTESIAN_POINT('Origin',(0.993747566553533,0.,-0.721999869202979));
#26329=CARTESIAN_POINT('',(1.08708260743774,0.,-0.612662169561028));
#26330=CARTESIAN_POINT('Origin',(0.,0.,0.));
#26331=CARTESIAN_POINT('',(1.13462523166105,0.,-0.519354515801077));
#26332=CARTESIAN_POINT('Origin',(1.0944585482776,0.,-0.557654483764164));
#26333=CARTESIAN_POINT('',(1.16954029537568,0.,-0.43506209545009));
#26334=CARTESIAN_POINT('Origin',(0.,0.,0.));
#26335=CARTESIAN_POINT('',(1.20190105810224,0.,-0.33546590875611));
#26336=CARTESIAN_POINT('Origin',(1.1682203282434,0.,-0.379577794185951));
#26337=CARTESIAN_POINT('',(1.22320001975977,0.,-0.246749348660852));
#26338=CARTESIAN_POINT('Origin',(0.,0.,0.));
#26339=CARTESIAN_POINT('',(1.23958209161204,0.,-0.143317017690053));
#26340=CARTESIAN_POINT('Origin',(1.21321664662686,0.,-0.192154639568406));
#26341=CARTESIAN_POINT('',(1.24674050008925,0.,-0.052360813993451));
#26342=CARTESIAN_POINT('Origin',(0.,0.,0.));
#26343=CARTESIAN_POINT('',(1.24674050008925,0.,0.052360813993451));
#26344=CARTESIAN_POINT('Origin',(1.22833954473516,0.,0.));
#26345=CARTESIAN_POINT('Origin',(0.,0.,0.));
#26346=CARTESIAN_POINT('Origin',(0.,0.,0.));
#26347=CARTESIAN_POINT('',(-1.4,-0.1,1.71450551880629E-16));
#26348=CARTESIAN_POINT('Origin',(0.,-0.1,0.));
#26349=CARTESIAN_POINT('',(-1.4,0.,-1.71450551880629E-16));
#26350=CARTESIAN_POINT('Origin',(0.,-0.1,0.));
#26351=CARTESIAN_POINT('Origin',(0.,0.75,0.));
#26352=CARTESIAN_POINT('',(-1.4,0.75,1.71450551880629E-16));
#26353=CARTESIAN_POINT('Origin',(0.,0.75,0.));
#26354=CARTESIAN_POINT('',(1.22320001975977,0.75,0.246749348660852));
#26355=CARTESIAN_POINT('',(1.23958209161204,0.75,0.143317017690053));
#26356=CARTESIAN_POINT('Origin',(1.21321664662686,0.75,0.192154639568406));
#26357=CARTESIAN_POINT('',(1.24674050008925,0.75,0.052360813993448));
#26358=CARTESIAN_POINT('Origin',(0.,0.75,0.));
#26359=CARTESIAN_POINT('',(1.24674050008925,0.75,-0.052360813993448));
#26360=CARTESIAN_POINT('Origin',(1.22833954473516,0.75,0.));
#26361=CARTESIAN_POINT('',(1.23958209161204,0.75,-0.143317017690053));
#26362=CARTESIAN_POINT('Origin',(0.,0.75,0.));
#26363=CARTESIAN_POINT('',(1.22320001975977,0.75,-0.246749348660852));
#26364=CARTESIAN_POINT('Origin',(1.21321664662686,0.75,-0.192154639568406));
#26365=CARTESIAN_POINT('',(1.20190105810224,0.75,-0.335465908756113));
#26366=CARTESIAN_POINT('Origin',(0.,0.75,0.));
#26367=CARTESIAN_POINT('',(1.16954029537568,0.75,-0.435062095450087));
#26368=CARTESIAN_POINT('Origin',(1.1682203282434,0.75,-0.379577794185951));
#26369=CARTESIAN_POINT('',(1.13462523166105,0.75,-0.519354515801077));
#26370=CARTESIAN_POINT('Origin',(0.,0.75,0.));
#26371=CARTESIAN_POINT('',(1.08708260743774,0.75,-0.612662169561028));
#26372=CARTESIAN_POINT('Origin',(1.0944585482776,0.75,-0.557654483764164));
#26373=CARTESIAN_POINT('',(1.0394111664111,0.75,-0.690454891028201));
#26374=CARTESIAN_POINT('Origin',(0.,0.75,0.));
#26375=CARTESIAN_POINT('',(0.977857337884349,0.75,-0.775176467748211));
#26376=CARTESIAN_POINT('Origin',(0.993747566553533,0.75,-0.721999869202979));
#26377=CARTESIAN_POINT('',(0.918603348636233,0.75,-0.844553975349804));
#26378=CARTESIAN_POINT('Origin',(0.,0.75,0.));
#26379=CARTESIAN_POINT('',(0.844553975349804,0.75,-0.918603348636233));
#26380=CARTESIAN_POINT('Origin',(0.86856722168183,0.75,-0.86856722168183));
#26381=CARTESIAN_POINT('',(0.775176467748211,0.75,-0.977857337884349));
#26382=CARTESIAN_POINT('Origin',(0.,0.75,0.));
#26383=CARTESIAN_POINT('',(0.690454891028201,0.75,-1.0394111664111));
#26384=CARTESIAN_POINT('Origin',(0.721999869202979,0.75,-0.993747566553533));
#26385=CARTESIAN_POINT('',(0.612662169561028,0.75,-1.08708260743774));
#26386=CARTESIAN_POINT('Origin',(0.,0.75,0.));
#26387=CARTESIAN_POINT('',(0.519354515801077,0.75,-1.13462523166105));
#26388=CARTESIAN_POINT('Origin',(0.557654483764164,0.75,-1.0944585482776));
#26389=CARTESIAN_POINT('',(0.435062095450087,0.75,-1.16954029537568));
#26390=CARTESIAN_POINT('Origin',(0.,0.75,0.));
#26391=CARTESIAN_POINT('',(0.335465908756113,0.75,-1.20190105810224));
#26392=CARTESIAN_POINT('Origin',(0.379577794185951,0.75,-1.1682203282434));
#26393=CARTESIAN_POINT('',(0.246749348660852,0.75,-1.22320001975977));
#26394=CARTESIAN_POINT('Origin',(0.,0.75,0.));
#26395=CARTESIAN_POINT('',(0.143317017690053,0.75,-1.23958209161204));
#26396=CARTESIAN_POINT('Origin',(0.192154639568406,0.75,-1.21321664662686));
#26397=CARTESIAN_POINT('',(0.0523608139934481,0.75,-1.24674050008925));
#26398=CARTESIAN_POINT('Origin',(0.,0.75,0.));
#26399=CARTESIAN_POINT('',(-0.0523608139934479,0.75,-1.24674050008925));
#26400=CARTESIAN_POINT('Origin',(7.52141045863017E-17,0.75,-1.22833954473516));
#26401=CARTESIAN_POINT('',(-0.143317017690053,0.75,-1.23958209161204));
#26402=CARTESIAN_POINT('Origin',(0.,0.75,0.));
#26403=CARTESIAN_POINT('',(-0.246749348660852,0.75,-1.22320001975977));
#26404=CARTESIAN_POINT('Origin',(-0.192154639568406,0.75,-1.21321664662686));
#26405=CARTESIAN_POINT('',(-0.335465908756113,0.75,-1.20190105810224));
#26406=CARTESIAN_POINT('Origin',(0.,0.75,0.));
#26407=CARTESIAN_POINT('',(-0.435062095450087,0.75,-1.16954029537568));
#26408=CARTESIAN_POINT('Origin',(-0.379577794185951,0.75,-1.1682203282434));
#26409=CARTESIAN_POINT('',(-0.519354515801077,0.75,-1.13462523166105));
#26410=CARTESIAN_POINT('Origin',(0.,0.75,0.));
#26411=CARTESIAN_POINT('',(-0.612662169561028,0.75,-1.08708260743774));
#26412=CARTESIAN_POINT('Origin',(-0.557654483764164,0.75,-1.0944585482776));
#26413=CARTESIAN_POINT('',(-0.690454891028201,0.75,-1.0394111664111));
#26414=CARTESIAN_POINT('Origin',(0.,0.75,0.));
#26415=CARTESIAN_POINT('',(-0.775176467748211,0.75,-0.977857337884348));
#26416=CARTESIAN_POINT('Origin',(-0.721999869202979,0.75,-0.993747566553533));
#26417=CARTESIAN_POINT('',(-0.844553975349804,0.75,-0.918603348636233));
#26418=CARTESIAN_POINT('Origin',(0.,0.75,0.));
#26419=CARTESIAN_POINT('',(-0.918603348636233,0.75,-0.844553975349804));
#26420=CARTESIAN_POINT('Origin',(-0.86856722168183,0.75,-0.86856722168183));
#26421=CARTESIAN_POINT('',(-0.977857337884349,0.75,-0.775176467748211));
#26422=CARTESIAN_POINT('Origin',(0.,0.75,0.));
#26423=CARTESIAN_POINT('',(-1.0394111664111,0.75,-0.690454891028201));
#26424=CARTESIAN_POINT('Origin',(-0.993747566553533,0.75,-0.721999869202979));
#26425=CARTESIAN_POINT('',(-1.08708260743774,0.75,-0.612662169561029));
#26426=CARTESIAN_POINT('Origin',(0.,0.75,0.));
#26427=CARTESIAN_POINT('',(-1.13462523166105,0.75,-0.519354515801077));
#26428=CARTESIAN_POINT('Origin',(-1.0944585482776,0.75,-0.557654483764164));
#26429=CARTESIAN_POINT('',(-1.16954029537568,0.75,-0.435062095450087));
#26430=CARTESIAN_POINT('Origin',(0.,0.75,0.));
#26431=CARTESIAN_POINT('',(-1.20190105810224,0.75,-0.335465908756113));
#26432=CARTESIAN_POINT('Origin',(-1.1682203282434,0.75,-0.379577794185951));
#26433=CARTESIAN_POINT('',(-1.22320001975977,0.75,-0.246749348660852));
#26434=CARTESIAN_POINT('Origin',(0.,0.75,0.));
#26435=CARTESIAN_POINT('',(-1.23958209161204,0.75,-0.143317017690053));
#26436=CARTESIAN_POINT('Origin',(-1.21321664662686,0.75,-0.192154639568406));
#26437=CARTESIAN_POINT('',(-1.24674050008925,0.75,-0.0523608139934482));
#26438=CARTESIAN_POINT('Origin',(0.,0.75,0.));
#26439=CARTESIAN_POINT('',(-1.24674050008925,0.75,0.0523608139934479));
#26440=CARTESIAN_POINT('Origin',(-1.22833954473516,0.75,-1.50428209172603E-16));
#26441=CARTESIAN_POINT('',(-1.23958209161204,0.75,0.143317017690053));
#26442=CARTESIAN_POINT('Origin',(0.,0.75,0.));
#26443=CARTESIAN_POINT('',(-1.22320001975977,0.75,0.246749348660851));
#26444=CARTESIAN_POINT('Origin',(-1.21321664662686,0.75,0.192154639568406));
#26445=CARTESIAN_POINT('',(-1.20190105810224,0.75,0.335465908756113));
#26446=CARTESIAN_POINT('Origin',(0.,0.75,0.));
#26447=CARTESIAN_POINT('',(-1.16954029537568,0.75,0.435062095450087));
#26448=CARTESIAN_POINT('Origin',(-1.1682203282434,0.75,0.379577794185951));
#26449=CARTESIAN_POINT('',(-1.13462523166105,0.75,0.519354515801077));
#26450=CARTESIAN_POINT('Origin',(0.,0.75,0.));
#26451=CARTESIAN_POINT('',(-1.08708260743774,0.75,0.612662169561028));
#26452=CARTESIAN_POINT('Origin',(-1.0944585482776,0.75,0.557654483764164));
#26453=CARTESIAN_POINT('',(-1.0394111664111,0.75,0.690454891028201));
#26454=CARTESIAN_POINT('Origin',(0.,0.75,0.));
#26455=CARTESIAN_POINT('',(-0.977857337884348,0.75,0.775176467748211));
#26456=CARTESIAN_POINT('Origin',(-0.993747566553533,0.75,0.721999869202979));
#26457=CARTESIAN_POINT('',(-0.918603348636233,0.75,0.844553975349804));
#26458=CARTESIAN_POINT('Origin',(0.,0.75,0.));
#26459=CARTESIAN_POINT('',(-0.844553975349804,0.75,0.918603348636233));
#26460=CARTESIAN_POINT('Origin',(-0.86856722168183,0.75,0.86856722168183));
#26461=CARTESIAN_POINT('',(-0.775176467748211,0.75,0.977857337884349));
#26462=CARTESIAN_POINT('Origin',(0.,0.75,0.));
#26463=CARTESIAN_POINT('',(-0.690454891028201,0.75,1.0394111664111));
#26464=CARTESIAN_POINT('Origin',(-0.721999869202979,0.75,0.993747566553533));
#26465=CARTESIAN_POINT('',(-0.612662169561029,0.75,1.08708260743774));
#26466=CARTESIAN_POINT('Origin',(0.,0.75,0.));
#26467=CARTESIAN_POINT('',(-0.519354515801077,0.75,1.13462523166105));
#26468=CARTESIAN_POINT('Origin',(-0.557654483764164,0.75,1.0944585482776));
#26469=CARTESIAN_POINT('',(-0.435062095450087,0.75,1.16954029537568));
#26470=CARTESIAN_POINT('Origin',(0.,0.75,0.));
#26471=CARTESIAN_POINT('',(-0.335465908756113,0.75,1.20190105810224));
#26472=CARTESIAN_POINT('Origin',(-0.379577794185951,0.75,1.1682203282434));
#26473=CARTESIAN_POINT('',(-0.246749348660852,0.75,1.22320001975977));
#26474=CARTESIAN_POINT('Origin',(0.,0.75,0.));
#26475=CARTESIAN_POINT('',(-0.143317017690053,0.75,1.23958209161204));
#26476=CARTESIAN_POINT('Origin',(-0.192154639568406,0.75,1.21321664662686));
#26477=CARTESIAN_POINT('',(-0.0523608139934483,0.75,1.24674050008925));
#26478=CARTESIAN_POINT('Origin',(0.,0.75,0.));
#26479=CARTESIAN_POINT('',(0.0523608139934478,0.75,1.24674050008925));
#26480=CARTESIAN_POINT('Origin',(-2.25642313758905E-16,0.75,1.22833954473516));
#26481=CARTESIAN_POINT('',(0.143317017690053,0.75,1.23958209161204));
#26482=CARTESIAN_POINT('Origin',(0.,0.75,0.));
#26483=CARTESIAN_POINT('',(0.246749348660851,0.75,1.22320001975977));
#26484=CARTESIAN_POINT('Origin',(0.192154639568406,0.75,1.21321664662686));
#26485=CARTESIAN_POINT('',(0.335465908756113,0.75,1.20190105810224));
#26486=CARTESIAN_POINT('Origin',(0.,0.75,0.));
#26487=CARTESIAN_POINT('',(0.435062095450087,0.75,1.16954029537568));
#26488=CARTESIAN_POINT('Origin',(0.379577794185951,0.75,1.1682203282434));
#26489=CARTESIAN_POINT('',(0.519354515801077,0.75,1.13462523166105));
#26490=CARTESIAN_POINT('Origin',(0.,0.75,0.));
#26491=CARTESIAN_POINT('',(0.612662169561028,0.75,1.08708260743774));
#26492=CARTESIAN_POINT('Origin',(0.557654483764164,0.75,1.0944585482776));
#26493=CARTESIAN_POINT('',(0.690454891028201,0.75,1.0394111664111));
#26494=CARTESIAN_POINT('Origin',(0.,0.75,0.));
#26495=CARTESIAN_POINT('',(0.775176467748211,0.75,0.977857337884349));
#26496=CARTESIAN_POINT('Origin',(0.721999869202979,0.75,0.993747566553533));
#26497=CARTESIAN_POINT('',(0.844553975349804,0.75,0.918603348636233));
#26498=CARTESIAN_POINT('Origin',(0.,0.75,0.));
#26499=CARTESIAN_POINT('',(0.918603348636233,0.75,0.844553975349804));
#26500=CARTESIAN_POINT('Origin',(0.86856722168183,0.75,0.86856722168183));
#26501=CARTESIAN_POINT('',(0.977857337884349,0.75,0.775176467748211));
#26502=CARTESIAN_POINT('Origin',(0.,0.75,0.));
#26503=CARTESIAN_POINT('',(1.0394111664111,0.75,0.690454891028201));
#26504=CARTESIAN_POINT('Origin',(0.993747566553533,0.75,0.72199986920298));
#26505=CARTESIAN_POINT('',(1.08708260743774,0.75,0.612662169561029));
#26506=CARTESIAN_POINT('Origin',(0.,0.75,0.));
#26507=CARTESIAN_POINT('',(1.13462523166105,0.75,0.519354515801077));
#26508=CARTESIAN_POINT('Origin',(1.0944585482776,0.75,0.557654483764164));
#26509=CARTESIAN_POINT('',(1.16954029537568,0.75,0.435062095450087));
#26510=CARTESIAN_POINT('Origin',(0.,0.75,0.));
#26511=CARTESIAN_POINT('',(1.20190105810224,0.75,0.335465908756113));
#26512=CARTESIAN_POINT('Origin',(1.1682203282434,0.75,0.379577794185952));
#26513=CARTESIAN_POINT('Origin',(0.,0.75,0.));
#26514=CARTESIAN_POINT('Origin',(0.,0.75,0.));
#26515=CARTESIAN_POINT('',(-1.4,0.85,1.71450551880629E-16));
#26516=CARTESIAN_POINT('Origin',(0.,0.85,0.));
#26517=CARTESIAN_POINT('',(-1.4,0.75,1.71450551880629E-16));
#26518=CARTESIAN_POINT('Origin',(0.,0.85,0.));
#26519=CARTESIAN_POINT('Origin',(1.21321664662686,0.,0.192154639568406));
#26520=CARTESIAN_POINT('',(1.23958209161204,0.,0.14331701769005));
#26521=CARTESIAN_POINT('',(1.22320001975977,0.,0.246749348660855));
#26522=CARTESIAN_POINT('Origin',(0.,0.,0.));
#26523=CARTESIAN_POINT('',(1.20190105810224,0.,0.33546590875611));
#26524=CARTESIAN_POINT('Origin',(1.1682203282434,0.,0.379577794185952));
#26525=CARTESIAN_POINT('',(1.16954029537568,0.,0.43506209545009));
#26526=CARTESIAN_POINT('Origin',(0.,0.,0.));
#26527=CARTESIAN_POINT('',(1.13462523166105,0.,0.519354515801074));
#26528=CARTESIAN_POINT('Origin',(1.0944585482776,0.,0.557654483764164));
#26529=CARTESIAN_POINT('',(1.08708260743774,0.,0.612662169561031));
#26530=CARTESIAN_POINT('Origin',(0.,0.,0.));
#26531=CARTESIAN_POINT('',(1.03941116641111,0.,0.690454891028199));
#26532=CARTESIAN_POINT('Origin',(0.993747566553533,0.,0.72199986920298));
#26533=CARTESIAN_POINT('',(0.977857337884347,0.,0.775176467748214));
#26534=CARTESIAN_POINT('Origin',(0.,0.,0.));
#26535=CARTESIAN_POINT('',(0.918603348636235,0.,0.844553975349802));
#26536=CARTESIAN_POINT('Origin',(0.86856722168183,0.,0.86856722168183));
#26537=CARTESIAN_POINT('',(0.844553975349802,0.,0.918603348636235));
#26538=CARTESIAN_POINT('Origin',(0.,0.,0.));
#26539=CARTESIAN_POINT('',(0.775176467748213,0.,0.977857337884347));
#26540=CARTESIAN_POINT('Origin',(0.721999869202979,0.,0.993747566553533));
#26541=CARTESIAN_POINT('',(0.690454891028198,0.,1.03941116641111));
#26542=CARTESIAN_POINT('Origin',(0.,0.,0.));
#26543=CARTESIAN_POINT('',(0.612662169561031,0.,1.08708260743774));
#26544=CARTESIAN_POINT('Origin',(0.557654483764164,0.,1.0944585482776));
#26545=CARTESIAN_POINT('',(0.519354515801074,0.,1.13462523166105));
#26546=CARTESIAN_POINT('Origin',(0.,0.,0.));
#26547=CARTESIAN_POINT('',(0.43506209545009,0.,1.16954029537568));
#26548=CARTESIAN_POINT('Origin',(0.379577794185951,0.,1.1682203282434));
#26549=CARTESIAN_POINT('',(0.33546590875611,0.,1.20190105810224));
#26550=CARTESIAN_POINT('Origin',(0.,0.,0.));
#26551=CARTESIAN_POINT('',(0.246749348660854,0.,1.22320001975977));
#26552=CARTESIAN_POINT('Origin',(0.192154639568406,0.,1.21321664662686));
#26553=CARTESIAN_POINT('',(0.14331701769005,0.,1.23958209161204));
#26554=CARTESIAN_POINT('Origin',(0.,0.,0.));
#26555=CARTESIAN_POINT('',(0.0523608139934508,0.,1.24674050008925));
#26556=CARTESIAN_POINT('Origin',(-2.25642313758905E-16,0.,1.22833954473516));
#26557=CARTESIAN_POINT('',(-0.0523608139934513,0.,1.24674050008925));
#26558=CARTESIAN_POINT('Origin',(0.,0.,0.));
#26559=CARTESIAN_POINT('',(-0.14331701769005,0.,1.23958209161204));
#26560=CARTESIAN_POINT('Origin',(-0.192154639568406,0.,1.21321664662686));
#26561=CARTESIAN_POINT('',(-0.246749348660855,0.,1.22320001975977));
#26562=CARTESIAN_POINT('Origin',(0.,0.,0.));
#26563=CARTESIAN_POINT('',(-0.33546590875611,0.,1.20190105810224));
#26564=CARTESIAN_POINT('Origin',(-0.379577794185951,0.,1.1682203282434));
#26565=CARTESIAN_POINT('',(-0.43506209545009,0.,1.16954029537568));
#26566=CARTESIAN_POINT('Origin',(0.,0.,0.));
#26567=CARTESIAN_POINT('',(-0.519354515801074,0.,1.13462523166105));
#26568=CARTESIAN_POINT('Origin',(-0.557654483764164,0.,1.0944585482776));
#26569=CARTESIAN_POINT('',(-0.612662169561031,0.,1.08708260743774));
#26570=CARTESIAN_POINT('Origin',(0.,0.,0.));
#26571=CARTESIAN_POINT('',(-0.690454891028199,0.,1.03941116641111));
#26572=CARTESIAN_POINT('Origin',(-0.721999869202979,0.,0.993747566553533));
#26573=CARTESIAN_POINT('',(-0.775176467748213,0.,0.977857337884347));
#26574=CARTESIAN_POINT('Origin',(0.,0.,0.));
#26575=CARTESIAN_POINT('',(-0.844553975349802,0.,0.918603348636235));
#26576=CARTESIAN_POINT('Origin',(-0.86856722168183,0.,0.86856722168183));
#26577=CARTESIAN_POINT('',(-0.918603348636235,0.,0.844553975349802));
#26578=CARTESIAN_POINT('Origin',(0.,0.,0.));
#26579=CARTESIAN_POINT('',(-0.977857337884347,0.,0.775176467748213));
#26580=CARTESIAN_POINT('Origin',(-0.993747566553533,0.,0.721999869202979));
#26581=CARTESIAN_POINT('',(-1.03941116641111,0.,0.690454891028198));
#26582=CARTESIAN_POINT('Origin',(0.,0.,0.));
#26583=CARTESIAN_POINT('',(-1.08708260743774,0.,0.612662169561031));
#26584=CARTESIAN_POINT('Origin',(-1.0944585482776,0.,0.557654483764164));
#26585=CARTESIAN_POINT('',(-1.13462523166105,0.,0.519354515801074));
#26586=CARTESIAN_POINT('Origin',(0.,0.,0.));
#26587=CARTESIAN_POINT('',(-1.16954029537568,0.,0.43506209545009));
#26588=CARTESIAN_POINT('Origin',(-1.1682203282434,0.,0.379577794185951));
#26589=CARTESIAN_POINT('',(-1.20190105810224,0.,0.33546590875611));
#26590=CARTESIAN_POINT('Origin',(0.,0.,0.));
#26591=CARTESIAN_POINT('',(-1.22320001975977,0.,0.246749348660854));
#26592=CARTESIAN_POINT('Origin',(-1.21321664662686,0.,0.192154639568406));
#26593=CARTESIAN_POINT('',(-1.23958209161204,0.,0.14331701769005));
#26594=CARTESIAN_POINT('Origin',(0.,0.,0.));
#26595=CARTESIAN_POINT('',(-1.24674050008925,0.,0.0523608139934509));
#26596=CARTESIAN_POINT('Origin',(-1.22833954473516,0.,-1.50428209172603E-16));
#26597=CARTESIAN_POINT('',(-1.24674050008925,0.,-0.0523608139934512));
#26598=CARTESIAN_POINT('Origin',(0.,0.,0.));
#26599=CARTESIAN_POINT('',(-1.23958209161204,0.,-0.14331701769005));
#26600=CARTESIAN_POINT('Origin',(-1.21321664662686,0.,-0.192154639568406));
#26601=CARTESIAN_POINT('',(-1.22320001975977,0.,-0.246749348660855));
#26602=CARTESIAN_POINT('Origin',(0.,0.,0.));
#26603=CARTESIAN_POINT('',(-1.20190105810224,0.,-0.33546590875611));
#26604=CARTESIAN_POINT('Origin',(-1.1682203282434,0.,-0.379577794185951));
#26605=CARTESIAN_POINT('',(-1.16954029537568,0.,-0.43506209545009));
#26606=CARTESIAN_POINT('Origin',(0.,0.,0.));
#26607=CARTESIAN_POINT('',(-1.13462523166105,0.,-0.519354515801074));
#26608=CARTESIAN_POINT('Origin',(-1.0944585482776,0.,-0.557654483764164));
#26609=CARTESIAN_POINT('',(-1.08708260743774,0.,-0.612662169561031));
#26610=CARTESIAN_POINT('Origin',(0.,0.,0.));
#26611=CARTESIAN_POINT('',(-1.03941116641111,0.,-0.690454891028199));
#26612=CARTESIAN_POINT('Origin',(-0.993747566553533,0.,-0.721999869202979));
#26613=CARTESIAN_POINT('',(-0.977857337884347,0.,-0.775176467748213));
#26614=CARTESIAN_POINT('Origin',(0.,0.,0.));
#26615=CARTESIAN_POINT('',(-0.918603348636235,0.,-0.844553975349802));
#26616=CARTESIAN_POINT('Origin',(-0.86856722168183,0.,-0.86856722168183));
#26617=CARTESIAN_POINT('',(-0.844553975349802,0.,-0.918603348636235));
#26618=CARTESIAN_POINT('Origin',(0.,0.,0.));
#26619=CARTESIAN_POINT('',(-0.775176467748213,0.,-0.977857337884347));
#26620=CARTESIAN_POINT('Origin',(-0.721999869202979,0.,-0.993747566553533));
#26621=CARTESIAN_POINT('',(-0.690454891028198,0.,-1.03941116641111));
#26622=CARTESIAN_POINT('Origin',(0.,0.,0.));
#26623=CARTESIAN_POINT('',(-0.612662169561031,0.,-1.08708260743774));
#26624=CARTESIAN_POINT('Origin',(-0.557654483764164,0.,-1.0944585482776));
#26625=CARTESIAN_POINT('',(-0.519354515801074,0.,-1.13462523166105));
#26626=CARTESIAN_POINT('Origin',(0.,0.,0.));
#26627=CARTESIAN_POINT('',(-0.43506209545009,0.,-1.16954029537568));
#26628=CARTESIAN_POINT('Origin',(-0.379577794185951,0.,-1.1682203282434));
#26629=CARTESIAN_POINT('',(-0.33546590875611,0.,-1.20190105810224));
#26630=CARTESIAN_POINT('Origin',(0.,0.,0.));
#26631=CARTESIAN_POINT('',(-0.246749348660854,0.,-1.22320001975977));
#26632=CARTESIAN_POINT('Origin',(-0.192154639568406,0.,-1.21321664662686));
#26633=CARTESIAN_POINT('',(-0.14331701769005,0.,-1.23958209161204));
#26634=CARTESIAN_POINT('Origin',(0.,0.,0.));
#26635=CARTESIAN_POINT('',(-0.052360813993451,0.,-1.24674050008925));
#26636=CARTESIAN_POINT('Origin',(7.52141045863017E-17,0.,-1.22833954473516));
#26637=CARTESIAN_POINT('',(0.0523608139934511,0.,-1.24674050008925));
#26638=CARTESIAN_POINT('Origin',(0.,0.,0.));
#26639=CARTESIAN_POINT('',(0.14331701769005,0.,-1.23958209161204));
#26640=CARTESIAN_POINT('Origin',(0.192154639568406,0.,-1.21321664662686));
#26641=CARTESIAN_POINT('',(0.246749348660855,0.,-1.22320001975977));
#26642=CARTESIAN_POINT('Origin',(0.,0.,0.));
#26643=CARTESIAN_POINT('',(0.33546590875611,0.,-1.20190105810224));
#26644=CARTESIAN_POINT('Origin',(0.379577794185951,0.,-1.1682203282434));
#26645=CARTESIAN_POINT('',(0.43506209545009,0.,-1.16954029537568));
#26646=CARTESIAN_POINT('Origin',(0.,0.,0.));
#26647=CARTESIAN_POINT('',(0.519354515801074,0.,-1.13462523166105));
#26648=CARTESIAN_POINT('Origin',(0.557654483764164,0.,-1.0944585482776));
#26649=CARTESIAN_POINT('',(0.612662169561031,0.,-1.08708260743774));
#26650=CARTESIAN_POINT('Origin',(0.,0.,0.));
#26651=CARTESIAN_POINT('',(0.690454891028198,0.,-1.03941116641111));
#26652=CARTESIAN_POINT('Origin',(0.721999869202979,0.,-0.993747566553533));
#26653=CARTESIAN_POINT('',(0.775176467748213,0.,-0.977857337884347));
#26654=CARTESIAN_POINT('Origin',(0.,0.,0.));
#26655=CARTESIAN_POINT('',(0.844553975349802,0.,-0.918603348636235));
#26656=CARTESIAN_POINT('Origin',(0.86856722168183,0.,-0.86856722168183));
#26657=CARTESIAN_POINT('',(0.918603348636235,0.,-0.844553975349802));
#26658=CARTESIAN_POINT('Origin',(0.,0.,0.));
#26659=CARTESIAN_POINT('',(0.977857337884347,0.,-0.775176467748213));
#26660=CARTESIAN_POINT('Origin',(0.993747566553533,0.,-0.721999869202979));
#26661=CARTESIAN_POINT('',(1.03941116641111,0.,-0.690454891028198));
#26662=CARTESIAN_POINT('Origin',(0.,0.,0.));
#26663=CARTESIAN_POINT('',(1.08708260743774,0.,-0.612662169561031));
#26664=CARTESIAN_POINT('Origin',(1.0944585482776,0.,-0.557654483764164));
#26665=CARTESIAN_POINT('',(1.13462523166105,0.,-0.519354515801074));
#26666=CARTESIAN_POINT('Origin',(0.,0.,0.));
#26667=CARTESIAN_POINT('',(1.16954029537568,0.,-0.43506209545009));
#26668=CARTESIAN_POINT('Origin',(1.1682203282434,0.,-0.379577794185951));
#26669=CARTESIAN_POINT('',(1.20190105810224,0.,-0.33546590875611));
#26670=CARTESIAN_POINT('Origin',(0.,0.,0.));
#26671=CARTESIAN_POINT('',(1.22320001975977,0.,-0.246749348660855));
#26672=CARTESIAN_POINT('Origin',(1.21321664662686,0.,-0.192154639568406));
#26673=CARTESIAN_POINT('',(1.23958209161204,0.,-0.14331701769005));
#26674=CARTESIAN_POINT('Origin',(0.,0.,0.));
#26675=CARTESIAN_POINT('',(1.24674050008925,0.,0.052360813993451));
#26676=CARTESIAN_POINT('Origin',(1.22833954473516,0.,0.));
#26677=CARTESIAN_POINT('',(1.24674050008925,0.,-0.052360813993451));
#26678=CARTESIAN_POINT('Origin',(0.,0.,0.));
#26679=CARTESIAN_POINT('',(0.,0.,0.));
#26680=CARTESIAN_POINT('Origin',(0.3,0.4,0.));
#26681=CARTESIAN_POINT('',(-0.3,0.4,-3.67394039744206E-17));
#26682=CARTESIAN_POINT('Origin',(0.,0.4,0.));
#26683=CARTESIAN_POINT('Origin',(0.,0.375,0.));
#26684=CARTESIAN_POINT('',(-0.35,0.35,-4.28626379701573E-17));
#26685=CARTESIAN_POINT('Origin',(0.,0.35,0.));
#26686=CARTESIAN_POINT('',(-0.325,0.375,-3.9801020972289E-17));
#26687=CARTESIAN_POINT('Origin',(0.,0.19,0.));
#26688=CARTESIAN_POINT('',(-0.35,0.03,-4.28626379701574E-17));
#26689=CARTESIAN_POINT('Origin',(0.,0.03,0.));
#26690=CARTESIAN_POINT('',(-0.35,0.19,-4.28626379701574E-17));
#26691=CARTESIAN_POINT('Origin',(0.,0.0149999999999999,0.));
#26692=CARTESIAN_POINT('',(-0.32,-3.29597460435593E-17,-3.91886975727153E-17));
#26693=CARTESIAN_POINT('Origin',(0.,0.,0.));
#26694=CARTESIAN_POINT('',(-0.335,0.0149999999999999,-4.10256677714363E-17));
#26695=CARTESIAN_POINT('Origin',(0.22,0.,0.));
#26696=CARTESIAN_POINT('',(-0.22,-6.93889390390723E-18,-2.69422295812418E-17));
#26697=CARTESIAN_POINT('Origin',(0.,0.,0.));
#26698=CARTESIAN_POINT('Origin',(0.,-0.02,0.));
#26699=CARTESIAN_POINT('',(-0.1954,-0.0492,2.39295984553393E-17));
#26700=CARTESIAN_POINT('Origin',(0.,-0.0492,0.));
#26701=CARTESIAN_POINT('',(-0.21,-0.02,-2.57175827820944E-17));
#26702=CARTESIAN_POINT('Origin',(0.,-0.8,0.));
#26703=CARTESIAN_POINT('',(-0.1954,-1.5646,2.39295984553393E-17));
#26704=CARTESIAN_POINT('Origin',(0.,-1.5646,0.));
#26705=CARTESIAN_POINT('',(-0.1954,-0.8,-2.39295984553393E-17));
#26706=CARTESIAN_POINT('Origin',(0.,-1.58,0.));
#26707=CARTESIAN_POINT('',(-0.16,-1.6,-1.95943487863577E-17));
#26708=CARTESIAN_POINT('Origin',(0.,-1.6,0.));
#26709=CARTESIAN_POINT('',(-0.18,-1.58,-2.20436423846524E-17));
#26710=CARTESIAN_POINT('Origin',(0.,-1.6,0.));
#26711=CARTESIAN_POINT('Origin',(0.0866025403784439,-0.4,-0.15));
#26712=CARTESIAN_POINT('',(0.173205080756888,-0.4,0.));
#26713=CARTESIAN_POINT('',(0.0866025403784439,-0.4,-0.15));
#26714=CARTESIAN_POINT('',(0.173205080756888,-0.4,0.));
#26715=CARTESIAN_POINT('',(0.0866025403784439,-0.64,-0.15));
#26716=CARTESIAN_POINT('',(0.0866025403784439,-0.4,-0.15));
#26717=CARTESIAN_POINT('',(0.173205080756888,-0.64,0.));
#26718=CARTESIAN_POINT('',(0.173205080756888,-0.64,0.));
#26719=CARTESIAN_POINT('',(0.173205080756888,-0.4,0.));
#26720=CARTESIAN_POINT('Origin',(-0.0866025403784438,-0.4,-0.15));
#26721=CARTESIAN_POINT('',(-0.0866025403784438,-0.4,-0.15));
#26722=CARTESIAN_POINT('',(0.0866025403784439,-0.4,-0.15));
#26723=CARTESIAN_POINT('',(-0.0866025403784438,-0.64,-0.15));
#26724=CARTESIAN_POINT('',(-0.0866025403784438,-0.4,-0.15));
#26725=CARTESIAN_POINT('',(0.0866025403784439,-0.64,-0.15));
#26726=CARTESIAN_POINT('Origin',(-0.173205080756888,-0.4,-2.77555756156289E-17));
#26727=CARTESIAN_POINT('',(-0.173205080756888,-0.4,-2.12115047744981E-17));
#26728=CARTESIAN_POINT('',(-0.0866025403784438,-0.4,-0.15));
#26729=CARTESIAN_POINT('',(-0.173205080756888,-0.64,-2.77555756156289E-17));
#26730=CARTESIAN_POINT('',(-0.173205080756888,-0.4,-2.12115047744981E-17));
#26731=CARTESIAN_POINT('',(-0.0866025403784438,-0.64,-0.15));
#26732=CARTESIAN_POINT('Origin',(-0.0866025403784439,-0.4,0.15));
#26733=CARTESIAN_POINT('',(-0.0866025403784439,-0.4,0.15));
#26734=CARTESIAN_POINT('',(-0.173205080756888,-0.4,-2.12115047744981E-17));
#26735=CARTESIAN_POINT('',(-0.0866025403784439,-0.64,0.15));
#26736=CARTESIAN_POINT('',(-0.0866025403784439,-0.4,0.15));
#26737=CARTESIAN_POINT('',(-0.173205080756888,-0.64,-2.12115047744981E-17));
#26738=CARTESIAN_POINT('Origin',(0.0866025403784439,-0.4,0.15));
#26739=CARTESIAN_POINT('',(0.0866025403784439,-0.4,0.15));
#26740=CARTESIAN_POINT('',(-0.0866025403784439,-0.4,0.15));
#26741=CARTESIAN_POINT('',(0.0866025403784439,-0.64,0.15));
#26742=CARTESIAN_POINT('',(0.0866025403784439,-0.4,0.15));
#26743=CARTESIAN_POINT('',(-0.0866025403784439,-0.64,0.15));
#26744=CARTESIAN_POINT('Origin',(0.173205080756888,-0.4,0.));
#26745=CARTESIAN_POINT('',(0.0866025403784439,-0.4,0.15));
#26746=CARTESIAN_POINT('',(0.0866025403784439,-0.64,0.15));
#26747=CARTESIAN_POINT('Origin',(0.,-0.4,-2.77555756156289E-17));
#26748=CARTESIAN_POINT('Origin',(0.,-0.64,-2.77555756156289E-17));
#26749=CARTESIAN_POINT('',(0.,0.,0.));
#26750=CARTESIAN_POINT('',(0.,0.,0.));
#26751=CARTESIAN_POINT('',(0.,0.,0.));
#26752=CARTESIAN_POINT('',(0.,0.,0.));
#26753=CARTESIAN_POINT('',(0.,0.,0.));
#26754=CARTESIAN_POINT('',(0.,0.,0.));
#26755=CARTESIAN_POINT('',(0.,0.,0.));
#26756=CARTESIAN_POINT('',(0.,0.,0.));
#26757=CARTESIAN_POINT('',(0.,0.,0.));
#26758=CARTESIAN_POINT('',(0.,0.,0.));
#26759=CARTESIAN_POINT('',(0.,0.,0.));
#26760=CARTESIAN_POINT('',(0.,0.,0.));
#26761=CARTESIAN_POINT('',(0.,0.,0.));
#26762=CARTESIAN_POINT('',(0.,0.,0.));
#26763=CARTESIAN_POINT('',(0.,0.,0.));
#26764=CARTESIAN_POINT('',(0.,0.,0.));
#26765=CARTESIAN_POINT('',(0.,0.,0.));
#26766=CARTESIAN_POINT('',(0.,0.,0.));
#26767=CARTESIAN_POINT('',(0.,0.,0.));
#26768=CARTESIAN_POINT('',(0.,0.,0.));
#26769=CARTESIAN_POINT('',(0.,0.,0.));
#26770=CARTESIAN_POINT('',(0.,0.,0.));
#26771=CARTESIAN_POINT('',(0.,0.,0.));
#26772=CARTESIAN_POINT('',(0.,0.,0.));
#26773=CARTESIAN_POINT('',(0.,0.,0.));
#26774=CARTESIAN_POINT('',(0.,0.,0.));
#26775=CARTESIAN_POINT('',(0.,0.,0.));
#26776=CARTESIAN_POINT('',(-2.8,-1.,0.8));
#26777=CARTESIAN_POINT('',(-2.8,1.,0.8));
#26778=CARTESIAN_POINT('',(2.8,-1.,0.8));
#26779=CARTESIAN_POINT('',(2.8,1.,0.8));
#26780=CARTESIAN_POINT('',(0.,-0.9,7.));
#26781=CARTESIAN_POINT('',(0.,0.9,7.));
#26782=CARTESIAN_POINT('',(1.34350288425444,-2.1,8.34350288425444));
#26783=CARTESIAN_POINT('',(-1.34350288425444,-2.1,8.34350288425444));
#26784=CARTESIAN_POINT('',(-1.34350288425444,-2.1,5.65649711574556));
#26785=CARTESIAN_POINT('',(1.34350288425444,-2.1,5.65649711574556));
#26786=CARTESIAN_POINT('',(1.34350288425444,2.1,8.34350288425444));
#26787=CARTESIAN_POINT('',(-1.34350288425444,2.1,8.34350288425444));
#26788=CARTESIAN_POINT('',(-1.34350288425444,2.1,5.65649711574556));
#26789=CARTESIAN_POINT('',(1.34350288425444,2.1,5.65649711574556));
#26790=CARTESIAN_POINT('',(4.17091003018116,-1.,0.8));
#26791=CARTESIAN_POINT('',(4.17091003018116,1.,0.8));
#26792=CARTESIAN_POINT('',(9.77091003018116,-1.,0.8));
#26793=CARTESIAN_POINT('',(9.77091003018116,1.,0.8));
#26794=CARTESIAN_POINT('',(6.97091003018116,-0.9,7.));
#26795=CARTESIAN_POINT('',(6.97091003018116,0.9,7.));
#26796=CARTESIAN_POINT('',(8.38512359255425,-2.1,8.4142135623731));
#26797=CARTESIAN_POINT('',(5.55669646780806,-2.1,8.4142135623731));
#26798=CARTESIAN_POINT('',(5.55669646780806,-2.1,5.58578643762691));
#26799=CARTESIAN_POINT('',(8.38512359255425,-2.1,5.58578643762691));
#26800=CARTESIAN_POINT('',(8.38512359255425,1.7,8.4142135623731));
#26801=CARTESIAN_POINT('',(5.55669646780806,1.7,8.4142135623731));
#26802=CARTESIAN_POINT('',(5.55669646780806,1.7,5.58578643762691));
#26803=CARTESIAN_POINT('',(8.38512359255425,1.7,5.58578643762691));
#26804=CARTESIAN_POINT('',(1.17091003018116,2.5,1.2));
#26805=CARTESIAN_POINT('',(1.17091003018116,5.5,1.2));
#26806=CARTESIAN_POINT('',(12.7709100301812,2.5,1.2));
#26807=CARTESIAN_POINT('',(12.7709100301812,5.5,1.2));
#26808=CARTESIAN_POINT('',(6.97091003018116,4.,7.));
#26809=CARTESIAN_POINT('',(2.22091003018116,4.,4.87));
#26810=CARTESIAN_POINT('',(2.22091003018116,4.,5.03));
#26811=CARTESIAN_POINT('',(11.7209100301812,4.,4.87));
#26812=CARTESIAN_POINT('',(11.7209100301812,4.,5.03));
#26813=CARTESIAN_POINT('',(1.17091003018116,38.5,1.2));
#26814=CARTESIAN_POINT('',(1.17091003018116,41.5,1.2));
#26815=CARTESIAN_POINT('',(12.7709100301812,38.5,1.2));
#26816=CARTESIAN_POINT('',(12.7709100301812,41.5,1.2));
#26817=CARTESIAN_POINT('',(6.97091003018116,40.,7.));
#26818=CARTESIAN_POINT('',(2.22091003018116,40.,4.87));
#26819=CARTESIAN_POINT('',(2.22091003018116,40.,5.03));
#26820=CARTESIAN_POINT('',(11.7209100301812,40.,4.87));
#26821=CARTESIAN_POINT('',(11.7209100301812,40.,5.03));
#26822=CARTESIAN_POINT('',(-1.5,4.5,0.8));
#26823=CARTESIAN_POINT('',(-1.5,8.5,0.8));
#26824=CARTESIAN_POINT('',(-3.,-6.2,4.5));
#26825=CARTESIAN_POINT('',(-3.,-6.2,10.));
#26826=CARTESIAN_POINT('',(9.97091003018116,-6.2,4.5));
#26827=CARTESIAN_POINT('',(9.97091003018116,-6.2,10.));
#26828=CARTESIAN_POINT('',(0.,0.,0.));
#26829=CARTESIAN_POINT('Origin',(0.0721687836487032,0.,-0.125));
#26830=CARTESIAN_POINT('',(0.0721687836487032,0.,-0.125));
#26831=CARTESIAN_POINT('',(0.144337567297406,0.,0.));
#26832=CARTESIAN_POINT('',(0.117710979560879,0.,-0.0461186027918559));
#26833=CARTESIAN_POINT('',(0.0721687836487032,-0.25,-0.125));
#26834=CARTESIAN_POINT('',(0.0721687836487032,0.,-0.125));
#26835=CARTESIAN_POINT('',(0.144337567297406,-0.25,0.));
#26836=CARTESIAN_POINT('',(0.144337567297406,-0.25,0.));
#26837=CARTESIAN_POINT('',(0.144337567297406,0.,0.));
#26838=CARTESIAN_POINT('Origin',(-0.0721687836487032,0.,-0.125));
#26839=CARTESIAN_POINT('',(-0.0721687836487032,0.,-0.125));
#26840=CARTESIAN_POINT('',(0.0739156081756484,0.,-0.125));
#26841=CARTESIAN_POINT('',(-0.0721687836487032,-0.25,-0.125));
#26842=CARTESIAN_POINT('',(-0.0721687836487032,0.,-0.125));
#26843=CARTESIAN_POINT('',(0.0721687836487032,-0.25,-0.125));
#26844=CARTESIAN_POINT('Origin',(-0.144337567297406,0.,-4.16333634234434E-17));
#26845=CARTESIAN_POINT('',(-0.144337567297406,0.,-1.76762539787485E-17));
#26846=CARTESIAN_POINT('',(-0.0987953713852306,0.,-0.0788813972081442));
#26847=CARTESIAN_POINT('',(-0.144337567297406,-0.25,-2.77555756156289E-17));
#26848=CARTESIAN_POINT('',(-0.144337567297406,0.,-1.76762539787485E-17));
#26849=CARTESIAN_POINT('',(-0.0721687836487032,-0.25,-0.125));
#26850=CARTESIAN_POINT('Origin',(-0.0721687836487033,0.,0.125));
#26851=CARTESIAN_POINT('',(-0.0721687836487033,0.,0.125));
#26852=CARTESIAN_POINT('',(-0.0627109795608791,0.,0.141381397208144));
#26853=CARTESIAN_POINT('',(-0.0721687836487033,-0.25,0.125));
#26854=CARTESIAN_POINT('',(-0.0721687836487033,0.,0.125));
#26855=CARTESIAN_POINT('',(-0.144337567297406,-0.25,-1.76762539787485E-17));
#26856=CARTESIAN_POINT('Origin',(0.0721687836487032,0.,0.125));
#26857=CARTESIAN_POINT('',(0.0721687836487032,0.,0.125));
#26858=CARTESIAN_POINT('',(0.146084391824352,0.,0.125));
#26859=CARTESIAN_POINT('',(0.0721687836487032,-0.25,0.125));
#26860=CARTESIAN_POINT('',(0.0721687836487032,0.,0.125));
#26861=CARTESIAN_POINT('',(-0.0721687836487033,-0.25,0.125));
#26862=CARTESIAN_POINT('Origin',(0.144337567297406,0.,0.));
#26863=CARTESIAN_POINT('',(0.153795371385231,0.,-0.0163813972081441));
#26864=CARTESIAN_POINT('',(0.0721687836487032,-0.25,0.125));
#26865=CARTESIAN_POINT('Origin',(0.,-0.25,0.));
#26866=CARTESIAN_POINT('Origin',(0.22,0.,0.));
#26867=CARTESIAN_POINT('',(-0.22,-8.67361737988404E-18,-2.69422295812418E-17));
#26868=CARTESIAN_POINT('Origin',(0.,0.,0.));
#26869=CARTESIAN_POINT('Origin',(0.,-0.015,0.));
#26870=CARTESIAN_POINT('',(-0.24505,-0.02505,-3.00099698131059E-17));
#26871=CARTESIAN_POINT('Origin',(0.,-0.02505,0.));
#26872=CARTESIAN_POINT('',(-0.235,-0.015,-2.87791997799628E-17));
#26873=CARTESIAN_POINT('Origin',(0.,-0.3775,0.));
#26874=CARTESIAN_POINT('',(-0.24505,-0.72995,3.00099698131059E-17));
#26875=CARTESIAN_POINT('Origin',(0.,-0.72995,0.));
#26876=CARTESIAN_POINT('',(-0.24505,-0.3775,-3.00099698131059E-17));
#26877=CARTESIAN_POINT('Origin',(0.,-0.7625,0.));
#26878=CARTESIAN_POINT('',(-0.175,-0.8,-2.14313189850787E-17));
#26879=CARTESIAN_POINT('Origin',(0.,-0.8,0.));
#26880=CARTESIAN_POINT('',(-0.2125,-0.7625,-2.60237444818813E-17));
#26881=CARTESIAN_POINT('Origin',(0.,-0.8,0.));
#26882=CARTESIAN_POINT('',(0.,0.,0.));
#26883=CARTESIAN_POINT('',(0.,0.,0.));
#26884=CARTESIAN_POINT('',(0.,0.,0.));
#26885=CARTESIAN_POINT('',(0.,0.,0.));
#26886=CARTESIAN_POINT('',(0.,0.,0.));
#26887=CARTESIAN_POINT('',(0.,0.,0.));
#26888=CARTESIAN_POINT('',(0.,0.,0.));
#26889=CARTESIAN_POINT('',(0.,0.,0.));
#26890=CARTESIAN_POINT('',(0.,-3.5,7.));
#26891=CARTESIAN_POINT('',(0.,-5.2,7.));
#26892=CARTESIAN_POINT('',(0.,2.5,8.3));
#26893=CARTESIAN_POINT('',(0.,3.5,8.3));
#26894=CARTESIAN_POINT('',(0.,0.,0.));
#26895=CARTESIAN_POINT('',(0.,0.,0.));
#26896=CARTESIAN_POINT('',(0.,0.,0.));
#26897=CARTESIAN_POINT('',(0.,0.,0.));
#26898=CARTESIAN_POINT('',(0.,0.,0.));
#26899=CARTESIAN_POINT('',(0.,0.,0.));
#26900=CARTESIAN_POINT('',(0.,0.,0.));
#26901=CARTESIAN_POINT('',(0.,0.,0.));
#26902=CARTESIAN_POINT('',(0.,0.,0.));
#26903=CARTESIAN_POINT('',(0.,0.,0.));
#26904=CARTESIAN_POINT('',(0.,0.,0.));
#26905=CARTESIAN_POINT('',(0.,0.,0.));
#26906=CARTESIAN_POINT('',(0.,0.,0.));
#26907=CARTESIAN_POINT('',(6.97091003018116,-3.5,7.));
#26908=CARTESIAN_POINT('',(6.97091003018116,-5.2,7.));
#26909=CARTESIAN_POINT('',(6.97091003018116,2.75,8.8));
#26910=CARTESIAN_POINT('',(6.97091003018116,42.85,8.8));
#26911=CARTESIAN_POINT('',(6.97091003018116,7.6,8.8));
#26912=CARTESIAN_POINT('',(6.97091003018116,36.4,8.8));
#26913=CARTESIAN_POINT('',(0.,0.,0.));
#26914=CARTESIAN_POINT('',(0.,0.,0.));
#26915=CARTESIAN_POINT('',(0.,0.,0.));
#26916=UNCERTAINTY_MEASURE_WITH_UNIT(LENGTH_MEASURE(0.001),#27070,
'DISTANCE_ACCURACY_VALUE',
'Maximum model space distance between geometric entities at asserted c
onnectivities');
#26917=UNCERTAINTY_MEASURE_WITH_UNIT(LENGTH_MEASURE(0.001),#27070,
'DISTANCE_ACCURACY_VALUE',
'Maximum model space distance between geometric entities at asserted c
onnectivities');
#26918=UNCERTAINTY_MEASURE_WITH_UNIT(LENGTH_MEASURE(0.001),#27070,
'DISTANCE_ACCURACY_VALUE',
'Maximum model space distance between geometric entities at asserted c
onnectivities');
#26919=UNCERTAINTY_MEASURE_WITH_UNIT(LENGTH_MEASURE(0.001),#27070,
'DISTANCE_ACCURACY_VALUE',
'Maximum model space distance between geometric entities at asserted c
onnectivities');
#26920=UNCERTAINTY_MEASURE_WITH_UNIT(LENGTH_MEASURE(0.001),#27070,
'DISTANCE_ACCURACY_VALUE',
'Maximum model space distance between geometric entities at asserted c
onnectivities');
#26921=UNCERTAINTY_MEASURE_WITH_UNIT(LENGTH_MEASURE(0.001),#27070,
'DISTANCE_ACCURACY_VALUE',
'Maximum model space distance between geometric entities at asserted c
onnectivities');
#26922=UNCERTAINTY_MEASURE_WITH_UNIT(LENGTH_MEASURE(0.001),#27070,
'DISTANCE_ACCURACY_VALUE',
'Maximum model space distance between geometric entities at asserted c
onnectivities');
#26923=UNCERTAINTY_MEASURE_WITH_UNIT(LENGTH_MEASURE(0.001),#27070,
'DISTANCE_ACCURACY_VALUE',
'Maximum model space distance between geometric entities at asserted c
onnectivities');
#26924=UNCERTAINTY_MEASURE_WITH_UNIT(LENGTH_MEASURE(0.001),#27070,
'DISTANCE_ACCURACY_VALUE',
'Maximum model space distance between geometric entities at asserted c
onnectivities');
#26925=UNCERTAINTY_MEASURE_WITH_UNIT(LENGTH_MEASURE(0.001),#27070,
'DISTANCE_ACCURACY_VALUE',
'Maximum model space distance between geometric entities at asserted c
onnectivities');
#26926=UNCERTAINTY_MEASURE_WITH_UNIT(LENGTH_MEASURE(0.001),#27070,
'DISTANCE_ACCURACY_VALUE',
'Maximum model space distance between geometric entities at asserted c
onnectivities');
#26927=UNCERTAINTY_MEASURE_WITH_UNIT(LENGTH_MEASURE(0.001),#27070,
'DISTANCE_ACCURACY_VALUE',
'Maximum model space distance between geometric entities at asserted c
onnectivities');
#26928=UNCERTAINTY_MEASURE_WITH_UNIT(LENGTH_MEASURE(0.001),#27070,
'DISTANCE_ACCURACY_VALUE',
'Maximum model space distance between geometric entities at asserted c
onnectivities');
#26929=UNCERTAINTY_MEASURE_WITH_UNIT(LENGTH_MEASURE(0.001),#27070,
'DISTANCE_ACCURACY_VALUE',
'Maximum model space distance between geometric entities at asserted c
onnectivities');
#26930=UNCERTAINTY_MEASURE_WITH_UNIT(LENGTH_MEASURE(0.001),#27070,
'DISTANCE_ACCURACY_VALUE',
'Maximum model space distance between geometric entities at asserted c
onnectivities');
#26931=UNCERTAINTY_MEASURE_WITH_UNIT(LENGTH_MEASURE(0.001),#27070,
'DISTANCE_ACCURACY_VALUE',
'Maximum model space distance between geometric entities at asserted c
onnectivities');
#26932=UNCERTAINTY_MEASURE_WITH_UNIT(LENGTH_MEASURE(0.001),#27070,
'DISTANCE_ACCURACY_VALUE',
'Maximum model space distance between geometric entities at asserted c
onnectivities');
#26933=UNCERTAINTY_MEASURE_WITH_UNIT(LENGTH_MEASURE(0.001),#27070,
'DISTANCE_ACCURACY_VALUE',
'Maximum model space distance between geometric entities at asserted c
onnectivities');
#26934=UNCERTAINTY_MEASURE_WITH_UNIT(LENGTH_MEASURE(0.001),#27070,
'DISTANCE_ACCURACY_VALUE',
'Maximum model space distance between geometric entities at asserted c
onnectivities');
#26935=UNCERTAINTY_MEASURE_WITH_UNIT(LENGTH_MEASURE(0.001),#27070,
'DISTANCE_ACCURACY_VALUE',
'Maximum model space distance between geometric entities at asserted c
onnectivities');
#26936=UNCERTAINTY_MEASURE_WITH_UNIT(LENGTH_MEASURE(0.001),#27070,
'DISTANCE_ACCURACY_VALUE',
'Maximum model space distance between geometric entities at asserted c
onnectivities');
#26937=UNCERTAINTY_MEASURE_WITH_UNIT(LENGTH_MEASURE(0.001),#27070,
'DISTANCE_ACCURACY_VALUE',
'Maximum model space distance between geometric entities at asserted c
onnectivities');
#26938=UNCERTAINTY_MEASURE_WITH_UNIT(LENGTH_MEASURE(0.001),#27070,
'DISTANCE_ACCURACY_VALUE',
'Maximum model space distance between geometric entities at asserted c
onnectivities');
#26939=UNCERTAINTY_MEASURE_WITH_UNIT(LENGTH_MEASURE(0.001),#27070,
'DISTANCE_ACCURACY_VALUE',
'Maximum model space distance between geometric entities at asserted c
onnectivities');
#26940=UNCERTAINTY_MEASURE_WITH_UNIT(LENGTH_MEASURE(0.001),#27070,
'DISTANCE_ACCURACY_VALUE',
'Maximum model space distance between geometric entities at asserted c
onnectivities');
#26941=UNCERTAINTY_MEASURE_WITH_UNIT(LENGTH_MEASURE(0.001),#27070,
'DISTANCE_ACCURACY_VALUE',
'Maximum model space distance between geometric entities at asserted c
onnectivities');
#26942=UNCERTAINTY_MEASURE_WITH_UNIT(LENGTH_MEASURE(0.001),#27070,
'DISTANCE_ACCURACY_VALUE',
'Maximum model space distance between geometric entities at asserted c
onnectivities');
#26943=UNCERTAINTY_MEASURE_WITH_UNIT(LENGTH_MEASURE(0.001),#27070,
'DISTANCE_ACCURACY_VALUE',
'Maximum model space distance between geometric entities at asserted c
onnectivities');
#26944=UNCERTAINTY_MEASURE_WITH_UNIT(LENGTH_MEASURE(0.001),#27070,
'DISTANCE_ACCURACY_VALUE',
'Maximum model space distance between geometric entities at asserted c
onnectivities');
#26945=UNCERTAINTY_MEASURE_WITH_UNIT(LENGTH_MEASURE(0.001),#27070,
'DISTANCE_ACCURACY_VALUE',
'Maximum model space distance between geometric entities at asserted c
onnectivities');
#26946=UNCERTAINTY_MEASURE_WITH_UNIT(LENGTH_MEASURE(0.001),#27070,
'DISTANCE_ACCURACY_VALUE',
'Maximum model space distance between geometric entities at asserted c
onnectivities');
#26947=UNCERTAINTY_MEASURE_WITH_UNIT(LENGTH_MEASURE(0.001),#27070,
'DISTANCE_ACCURACY_VALUE',
'Maximum model space distance between geometric entities at asserted c
onnectivities');
#26948=UNCERTAINTY_MEASURE_WITH_UNIT(LENGTH_MEASURE(0.001),#27070,
'DISTANCE_ACCURACY_VALUE',
'Maximum model space distance between geometric entities at asserted c
onnectivities');
#26949=UNCERTAINTY_MEASURE_WITH_UNIT(LENGTH_MEASURE(0.001),#27070,
'DISTANCE_ACCURACY_VALUE',
'Maximum model space distance between geometric entities at asserted c
onnectivities');
#26950=UNCERTAINTY_MEASURE_WITH_UNIT(LENGTH_MEASURE(0.001),#27070,
'DISTANCE_ACCURACY_VALUE',
'Maximum model space distance between geometric entities at asserted c
onnectivities');
#26951=UNCERTAINTY_MEASURE_WITH_UNIT(LENGTH_MEASURE(0.001),#27070,
'DISTANCE_ACCURACY_VALUE',
'Maximum model space distance between geometric entities at asserted c
onnectivities');
#26952=UNCERTAINTY_MEASURE_WITH_UNIT(LENGTH_MEASURE(0.001),#27070,
'DISTANCE_ACCURACY_VALUE',
'Maximum model space distance between geometric entities at asserted c
onnectivities');
#26953=UNCERTAINTY_MEASURE_WITH_UNIT(LENGTH_MEASURE(0.001),#27070,
'DISTANCE_ACCURACY_VALUE',
'Maximum model space distance between geometric entities at asserted c
onnectivities');
#26954=UNCERTAINTY_MEASURE_WITH_UNIT(LENGTH_MEASURE(0.001),#27070,
'DISTANCE_ACCURACY_VALUE',
'Maximum model space distance between geometric entities at asserted c
onnectivities');
#26955=UNCERTAINTY_MEASURE_WITH_UNIT(LENGTH_MEASURE(0.001),#27070,
'DISTANCE_ACCURACY_VALUE',
'Maximum model space distance between geometric entities at asserted c
onnectivities');
#26956=UNCERTAINTY_MEASURE_WITH_UNIT(LENGTH_MEASURE(0.001),#27070,
'DISTANCE_ACCURACY_VALUE',
'Maximum model space distance between geometric entities at asserted c
onnectivities');
#26957=UNCERTAINTY_MEASURE_WITH_UNIT(LENGTH_MEASURE(0.001),#27070,
'DISTANCE_ACCURACY_VALUE',
'Maximum model space distance between geometric entities at asserted c
onnectivities');
#26958=UNCERTAINTY_MEASURE_WITH_UNIT(LENGTH_MEASURE(0.001),#27070,
'DISTANCE_ACCURACY_VALUE',
'Maximum model space distance between geometric entities at asserted c
onnectivities');
#26959=UNCERTAINTY_MEASURE_WITH_UNIT(LENGTH_MEASURE(0.001),#27070,
'DISTANCE_ACCURACY_VALUE',
'Maximum model space distance between geometric entities at asserted c
onnectivities');
#26960=UNCERTAINTY_MEASURE_WITH_UNIT(LENGTH_MEASURE(0.001),#27070,
'DISTANCE_ACCURACY_VALUE',
'Maximum model space distance between geometric entities at asserted c
onnectivities');
#26961=UNCERTAINTY_MEASURE_WITH_UNIT(LENGTH_MEASURE(0.001),#27070,
'DISTANCE_ACCURACY_VALUE',
'Maximum model space distance between geometric entities at asserted c
onnectivities');
#26962=UNCERTAINTY_MEASURE_WITH_UNIT(LENGTH_MEASURE(0.001),#27070,
'DISTANCE_ACCURACY_VALUE',
'Maximum model space distance between geometric entities at asserted c
onnectivities');
#26963=UNCERTAINTY_MEASURE_WITH_UNIT(LENGTH_MEASURE(0.001),#27070,
'DISTANCE_ACCURACY_VALUE',
'Maximum model space distance between geometric entities at asserted c
onnectivities');
#26964=UNCERTAINTY_MEASURE_WITH_UNIT(LENGTH_MEASURE(0.001),#27070,
'DISTANCE_ACCURACY_VALUE',
'Maximum model space distance between geometric entities at asserted c
onnectivities');
#26965=UNCERTAINTY_MEASURE_WITH_UNIT(LENGTH_MEASURE(0.001),#27070,
'DISTANCE_ACCURACY_VALUE',
'Maximum model space distance between geometric entities at asserted c
onnectivities');
#26966=UNCERTAINTY_MEASURE_WITH_UNIT(LENGTH_MEASURE(0.001),#27070,
'DISTANCE_ACCURACY_VALUE',
'Maximum model space distance between geometric entities at asserted c
onnectivities');
#26967=UNCERTAINTY_MEASURE_WITH_UNIT(LENGTH_MEASURE(0.001),#27070,
'DISTANCE_ACCURACY_VALUE',
'Maximum model space distance between geometric entities at asserted c
onnectivities');
#26968=UNCERTAINTY_MEASURE_WITH_UNIT(LENGTH_MEASURE(0.001),#27070,
'DISTANCE_ACCURACY_VALUE',
'Maximum model space distance between geometric entities at asserted c
onnectivities');
#26969=UNCERTAINTY_MEASURE_WITH_UNIT(LENGTH_MEASURE(0.001),#27070,
'DISTANCE_ACCURACY_VALUE',
'Maximum model space distance between geometric entities at asserted c
onnectivities');
#26970=UNCERTAINTY_MEASURE_WITH_UNIT(LENGTH_MEASURE(0.001),#27070,
'DISTANCE_ACCURACY_VALUE',
'Maximum model space distance between geometric entities at asserted c
onnectivities');
#26971=UNCERTAINTY_MEASURE_WITH_UNIT(LENGTH_MEASURE(0.001),#27070,
'DISTANCE_ACCURACY_VALUE',
'Maximum model space distance between geometric entities at asserted c
onnectivities');
#26972=UNCERTAINTY_MEASURE_WITH_UNIT(LENGTH_MEASURE(0.001),#27070,
'DISTANCE_ACCURACY_VALUE',
'Maximum model space distance between geometric entities at asserted c
onnectivities');
#26973=UNCERTAINTY_MEASURE_WITH_UNIT(LENGTH_MEASURE(0.001),#27070,
'DISTANCE_ACCURACY_VALUE',
'Maximum model space distance between geometric entities at asserted c
onnectivities');
#26974=UNCERTAINTY_MEASURE_WITH_UNIT(LENGTH_MEASURE(0.001),#27070,
'DISTANCE_ACCURACY_VALUE',
'Maximum model space distance between geometric entities at asserted c
onnectivities');
#26975=UNCERTAINTY_MEASURE_WITH_UNIT(LENGTH_MEASURE(0.001),#27070,
'DISTANCE_ACCURACY_VALUE',
'Maximum model space distance between geometric entities at asserted c
onnectivities');
#26976=UNCERTAINTY_MEASURE_WITH_UNIT(LENGTH_MEASURE(0.001),#27070,
'DISTANCE_ACCURACY_VALUE',
'Maximum model space distance between geometric entities at asserted c
onnectivities');
#26977=UNCERTAINTY_MEASURE_WITH_UNIT(LENGTH_MEASURE(0.001),#27070,
'DISTANCE_ACCURACY_VALUE',
'Maximum model space distance between geometric entities at asserted c
onnectivities');
#26978=UNCERTAINTY_MEASURE_WITH_UNIT(LENGTH_MEASURE(0.001),#27070,
'DISTANCE_ACCURACY_VALUE',
'Maximum model space distance between geometric entities at asserted c
onnectivities');
#26979=UNCERTAINTY_MEASURE_WITH_UNIT(LENGTH_MEASURE(0.001),#27070,
'DISTANCE_ACCURACY_VALUE',
'Maximum model space distance between geometric entities at asserted c
onnectivities');
#26980=UNCERTAINTY_MEASURE_WITH_UNIT(LENGTH_MEASURE(0.001),#27070,
'DISTANCE_ACCURACY_VALUE',
'Maximum model space distance between geometric entities at asserted c
onnectivities');
#26981=UNCERTAINTY_MEASURE_WITH_UNIT(LENGTH_MEASURE(0.001),#27070,
'DISTANCE_ACCURACY_VALUE',
'Maximum model space distance between geometric entities at asserted c
onnectivities');
#26982=UNCERTAINTY_MEASURE_WITH_UNIT(LENGTH_MEASURE(0.001),#27070,
'DISTANCE_ACCURACY_VALUE',
'Maximum model space distance between geometric entities at asserted c
onnectivities');
#26983=UNCERTAINTY_MEASURE_WITH_UNIT(LENGTH_MEASURE(0.001),#27070,
'DISTANCE_ACCURACY_VALUE',
'Maximum model space distance between geometric entities at asserted c
onnectivities');
#26984=UNCERTAINTY_MEASURE_WITH_UNIT(LENGTH_MEASURE(0.001),#27070,
'DISTANCE_ACCURACY_VALUE',
'Maximum model space distance between geometric entities at asserted c
onnectivities');
#26985=UNCERTAINTY_MEASURE_WITH_UNIT(LENGTH_MEASURE(0.001),#27070,
'DISTANCE_ACCURACY_VALUE',
'Maximum model space distance between geometric entities at asserted c
onnectivities');
#26986=UNCERTAINTY_MEASURE_WITH_UNIT(LENGTH_MEASURE(0.001),#27070,
'DISTANCE_ACCURACY_VALUE',
'Maximum model space distance between geometric entities at asserted c
onnectivities');
#26987=UNCERTAINTY_MEASURE_WITH_UNIT(LENGTH_MEASURE(0.001),#27070,
'DISTANCE_ACCURACY_VALUE',
'Maximum model space distance between geometric entities at asserted c
onnectivities');
#26988=UNCERTAINTY_MEASURE_WITH_UNIT(LENGTH_MEASURE(0.001),#27070,
'DISTANCE_ACCURACY_VALUE',
'Maximum model space distance between geometric entities at asserted c
onnectivities');
#26989=UNCERTAINTY_MEASURE_WITH_UNIT(LENGTH_MEASURE(0.001),#27070,
'DISTANCE_ACCURACY_VALUE',
'Maximum model space distance between geometric entities at asserted c
onnectivities');
#26990=UNCERTAINTY_MEASURE_WITH_UNIT(LENGTH_MEASURE(0.001),#27070,
'DISTANCE_ACCURACY_VALUE',
'Maximum model space distance between geometric entities at asserted c
onnectivities');
#26991=UNCERTAINTY_MEASURE_WITH_UNIT(LENGTH_MEASURE(0.001),#27070,
'DISTANCE_ACCURACY_VALUE',
'Maximum model space distance between geometric entities at asserted c
onnectivities');
#26992=UNCERTAINTY_MEASURE_WITH_UNIT(LENGTH_MEASURE(0.001),#27070,
'DISTANCE_ACCURACY_VALUE',
'Maximum model space distance between geometric entities at asserted c
onnectivities');
#26993=(
GEOMETRIC_REPRESENTATION_CONTEXT(3)
GLOBAL_UNCERTAINTY_ASSIGNED_CONTEXT((#26916))
GLOBAL_UNIT_ASSIGNED_CONTEXT((#27070,#27072,#27073))
REPRESENTATION_CONTEXT('','3D')
);
#26994=(
GEOMETRIC_REPRESENTATION_CONTEXT(3)
GLOBAL_UNCERTAINTY_ASSIGNED_CONTEXT((#26917))
GLOBAL_UNIT_ASSIGNED_CONTEXT((#27070,#27072,#27073))
REPRESENTATION_CONTEXT('','3D')
);
#26995=(
GEOMETRIC_REPRESENTATION_CONTEXT(3)
GLOBAL_UNCERTAINTY_ASSIGNED_CONTEXT((#26918))
GLOBAL_UNIT_ASSIGNED_CONTEXT((#27070,#27072,#27073))
REPRESENTATION_CONTEXT('','3D')
);
#26996=(
GEOMETRIC_REPRESENTATION_CONTEXT(3)
GLOBAL_UNCERTAINTY_ASSIGNED_CONTEXT((#26919))
GLOBAL_UNIT_ASSIGNED_CONTEXT((#27070,#27072,#27073))
REPRESENTATION_CONTEXT('','3D')
);
#26997=(
GEOMETRIC_REPRESENTATION_CONTEXT(3)
GLOBAL_UNCERTAINTY_ASSIGNED_CONTEXT((#26920))
GLOBAL_UNIT_ASSIGNED_CONTEXT((#27070,#27072,#27073))
REPRESENTATION_CONTEXT('','3D')
);
#26998=(
GEOMETRIC_REPRESENTATION_CONTEXT(3)
GLOBAL_UNCERTAINTY_ASSIGNED_CONTEXT((#26921))
GLOBAL_UNIT_ASSIGNED_CONTEXT((#27070,#27072,#27073))
REPRESENTATION_CONTEXT('','3D')
);
#26999=(
GEOMETRIC_REPRESENTATION_CONTEXT(3)
GLOBAL_UNCERTAINTY_ASSIGNED_CONTEXT((#26922))
GLOBAL_UNIT_ASSIGNED_CONTEXT((#27070,#27072,#27073))
REPRESENTATION_CONTEXT('','3D')
);
#27000=(
GEOMETRIC_REPRESENTATION_CONTEXT(3)
GLOBAL_UNCERTAINTY_ASSIGNED_CONTEXT((#26923))
GLOBAL_UNIT_ASSIGNED_CONTEXT((#27070,#27072,#27073))
REPRESENTATION_CONTEXT('','3D')
);
#27001=(
GEOMETRIC_REPRESENTATION_CONTEXT(3)
GLOBAL_UNCERTAINTY_ASSIGNED_CONTEXT((#26924))
GLOBAL_UNIT_ASSIGNED_CONTEXT((#27070,#27072,#27073))
REPRESENTATION_CONTEXT('','3D')
);
#27002=(
GEOMETRIC_REPRESENTATION_CONTEXT(3)
GLOBAL_UNCERTAINTY_ASSIGNED_CONTEXT((#26925))
GLOBAL_UNIT_ASSIGNED_CONTEXT((#27070,#27072,#27073))
REPRESENTATION_CONTEXT('','3D')
);
#27003=(
GEOMETRIC_REPRESENTATION_CONTEXT(3)
GLOBAL_UNCERTAINTY_ASSIGNED_CONTEXT((#26926))
GLOBAL_UNIT_ASSIGNED_CONTEXT((#27070,#27072,#27073))
REPRESENTATION_CONTEXT('','3D')
);
#27004=(
GEOMETRIC_REPRESENTATION_CONTEXT(3)
GLOBAL_UNCERTAINTY_ASSIGNED_CONTEXT((#26927))
GLOBAL_UNIT_ASSIGNED_CONTEXT((#27070,#27072,#27073))
REPRESENTATION_CONTEXT('','3D')
);
#27005=(
GEOMETRIC_REPRESENTATION_CONTEXT(3)
GLOBAL_UNCERTAINTY_ASSIGNED_CONTEXT((#26928))
GLOBAL_UNIT_ASSIGNED_CONTEXT((#27070,#27072,#27073))
REPRESENTATION_CONTEXT('','3D')
);
#27006=(
GEOMETRIC_REPRESENTATION_CONTEXT(3)
GLOBAL_UNCERTAINTY_ASSIGNED_CONTEXT((#26929))
GLOBAL_UNIT_ASSIGNED_CONTEXT((#27070,#27072,#27073))
REPRESENTATION_CONTEXT('','3D')
);
#27007=(
GEOMETRIC_REPRESENTATION_CONTEXT(3)
GLOBAL_UNCERTAINTY_ASSIGNED_CONTEXT((#26930))
GLOBAL_UNIT_ASSIGNED_CONTEXT((#27070,#27072,#27073))
REPRESENTATION_CONTEXT('','3D')
);
#27008=(
GEOMETRIC_REPRESENTATION_CONTEXT(3)
GLOBAL_UNCERTAINTY_ASSIGNED_CONTEXT((#26931))
GLOBAL_UNIT_ASSIGNED_CONTEXT((#27070,#27072,#27073))
REPRESENTATION_CONTEXT('','3D')
);
#27009=(
GEOMETRIC_REPRESENTATION_CONTEXT(3)
GLOBAL_UNCERTAINTY_ASSIGNED_CONTEXT((#26932))
GLOBAL_UNIT_ASSIGNED_CONTEXT((#27070,#27072,#27073))
REPRESENTATION_CONTEXT('','3D')
);
#27010=(
GEOMETRIC_REPRESENTATION_CONTEXT(3)
GLOBAL_UNCERTAINTY_ASSIGNED_CONTEXT((#26933))
GLOBAL_UNIT_ASSIGNED_CONTEXT((#27070,#27072,#27073))
REPRESENTATION_CONTEXT('','3D')
);
#27011=(
GEOMETRIC_REPRESENTATION_CONTEXT(3)
GLOBAL_UNCERTAINTY_ASSIGNED_CONTEXT((#26934))
GLOBAL_UNIT_ASSIGNED_CONTEXT((#27070,#27072,#27073))
REPRESENTATION_CONTEXT('','3D')
);
#27012=(
GEOMETRIC_REPRESENTATION_CONTEXT(3)
GLOBAL_UNCERTAINTY_ASSIGNED_CONTEXT((#26935))
GLOBAL_UNIT_ASSIGNED_CONTEXT((#27070,#27072,#27073))
REPRESENTATION_CONTEXT('','3D')
);
#27013=(
GEOMETRIC_REPRESENTATION_CONTEXT(3)
GLOBAL_UNCERTAINTY_ASSIGNED_CONTEXT((#26936))
GLOBAL_UNIT_ASSIGNED_CONTEXT((#27070,#27072,#27073))
REPRESENTATION_CONTEXT('','3D')
);
#27014=(
GEOMETRIC_REPRESENTATION_CONTEXT(3)
GLOBAL_UNCERTAINTY_ASSIGNED_CONTEXT((#26937))
GLOBAL_UNIT_ASSIGNED_CONTEXT((#27070,#27072,#27073))
REPRESENTATION_CONTEXT('','3D')
);
#27015=(
GEOMETRIC_REPRESENTATION_CONTEXT(3)
GLOBAL_UNCERTAINTY_ASSIGNED_CONTEXT((#26938))
GLOBAL_UNIT_ASSIGNED_CONTEXT((#27070,#27072,#27073))
REPRESENTATION_CONTEXT('','3D')
);
#27016=(
GEOMETRIC_REPRESENTATION_CONTEXT(3)
GLOBAL_UNCERTAINTY_ASSIGNED_CONTEXT((#26939))
GLOBAL_UNIT_ASSIGNED_CONTEXT((#27070,#27072,#27073))
REPRESENTATION_CONTEXT('','3D')
);
#27017=(
GEOMETRIC_REPRESENTATION_CONTEXT(3)
GLOBAL_UNCERTAINTY_ASSIGNED_CONTEXT((#26940))
GLOBAL_UNIT_ASSIGNED_CONTEXT((#27070,#27072,#27073))
REPRESENTATION_CONTEXT('','3D')
);
#27018=(
GEOMETRIC_REPRESENTATION_CONTEXT(3)
GLOBAL_UNCERTAINTY_ASSIGNED_CONTEXT((#26941))
GLOBAL_UNIT_ASSIGNED_CONTEXT((#27070,#27072,#27073))
REPRESENTATION_CONTEXT('','3D')
);
#27019=(
GEOMETRIC_REPRESENTATION_CONTEXT(3)
GLOBAL_UNCERTAINTY_ASSIGNED_CONTEXT((#26942))
GLOBAL_UNIT_ASSIGNED_CONTEXT((#27070,#27072,#27073))
REPRESENTATION_CONTEXT('','3D')
);
#27020=(
GEOMETRIC_REPRESENTATION_CONTEXT(3)
GLOBAL_UNCERTAINTY_ASSIGNED_CONTEXT((#26943))
GLOBAL_UNIT_ASSIGNED_CONTEXT((#27070,#27072,#27073))
REPRESENTATION_CONTEXT('','3D')
);
#27021=(
GEOMETRIC_REPRESENTATION_CONTEXT(3)
GLOBAL_UNCERTAINTY_ASSIGNED_CONTEXT((#26944))
GLOBAL_UNIT_ASSIGNED_CONTEXT((#27070,#27072,#27073))
REPRESENTATION_CONTEXT('','3D')
);
#27022=(
GEOMETRIC_REPRESENTATION_CONTEXT(3)
GLOBAL_UNCERTAINTY_ASSIGNED_CONTEXT((#26945))
GLOBAL_UNIT_ASSIGNED_CONTEXT((#27070,#27072,#27073))
REPRESENTATION_CONTEXT('','3D')
);
#27023=(
GEOMETRIC_REPRESENTATION_CONTEXT(3)
GLOBAL_UNCERTAINTY_ASSIGNED_CONTEXT((#26946))
GLOBAL_UNIT_ASSIGNED_CONTEXT((#27070,#27072,#27073))
REPRESENTATION_CONTEXT('','3D')
);
#27024=(
GEOMETRIC_REPRESENTATION_CONTEXT(3)
GLOBAL_UNCERTAINTY_ASSIGNED_CONTEXT((#26947))
GLOBAL_UNIT_ASSIGNED_CONTEXT((#27070,#27072,#27073))
REPRESENTATION_CONTEXT('','3D')
);
#27025=(
GEOMETRIC_REPRESENTATION_CONTEXT(3)
GLOBAL_UNCERTAINTY_ASSIGNED_CONTEXT((#26948))
GLOBAL_UNIT_ASSIGNED_CONTEXT((#27070,#27072,#27073))
REPRESENTATION_CONTEXT('','3D')
);
#27026=(
GEOMETRIC_REPRESENTATION_CONTEXT(3)
GLOBAL_UNCERTAINTY_ASSIGNED_CONTEXT((#26949))
GLOBAL_UNIT_ASSIGNED_CONTEXT((#27070,#27072,#27073))
REPRESENTATION_CONTEXT('','3D')
);
#27027=(
GEOMETRIC_REPRESENTATION_CONTEXT(3)
GLOBAL_UNCERTAINTY_ASSIGNED_CONTEXT((#26950))
GLOBAL_UNIT_ASSIGNED_CONTEXT((#27070,#27072,#27073))
REPRESENTATION_CONTEXT('','3D')
);
#27028=(
GEOMETRIC_REPRESENTATION_CONTEXT(3)
GLOBAL_UNCERTAINTY_ASSIGNED_CONTEXT((#26951))
GLOBAL_UNIT_ASSIGNED_CONTEXT((#27070,#27072,#27073))
REPRESENTATION_CONTEXT('','3D')
);
#27029=(
GEOMETRIC_REPRESENTATION_CONTEXT(3)
GLOBAL_UNCERTAINTY_ASSIGNED_CONTEXT((#26952))
GLOBAL_UNIT_ASSIGNED_CONTEXT((#27070,#27072,#27073))
REPRESENTATION_CONTEXT('','3D')
);
#27030=(
GEOMETRIC_REPRESENTATION_CONTEXT(3)
GLOBAL_UNCERTAINTY_ASSIGNED_CONTEXT((#26953))
GLOBAL_UNIT_ASSIGNED_CONTEXT((#27070,#27072,#27073))
REPRESENTATION_CONTEXT('','3D')
);
#27031=(
GEOMETRIC_REPRESENTATION_CONTEXT(3)
GLOBAL_UNCERTAINTY_ASSIGNED_CONTEXT((#26954))
GLOBAL_UNIT_ASSIGNED_CONTEXT((#27070,#27072,#27073))
REPRESENTATION_CONTEXT('','3D')
);
#27032=(
GEOMETRIC_REPRESENTATION_CONTEXT(3)
GLOBAL_UNCERTAINTY_ASSIGNED_CONTEXT((#26955))
GLOBAL_UNIT_ASSIGNED_CONTEXT((#27070,#27072,#27073))
REPRESENTATION_CONTEXT('','3D')
);
#27033=(
GEOMETRIC_REPRESENTATION_CONTEXT(3)
GLOBAL_UNCERTAINTY_ASSIGNED_CONTEXT((#26956))
GLOBAL_UNIT_ASSIGNED_CONTEXT((#27070,#27072,#27073))
REPRESENTATION_CONTEXT('','3D')
);
#27034=(
GEOMETRIC_REPRESENTATION_CONTEXT(3)
GLOBAL_UNCERTAINTY_ASSIGNED_CONTEXT((#26957))
GLOBAL_UNIT_ASSIGNED_CONTEXT((#27070,#27072,#27073))
REPRESENTATION_CONTEXT('','3D')
);
#27035=(
GEOMETRIC_REPRESENTATION_CONTEXT(3)
GLOBAL_UNCERTAINTY_ASSIGNED_CONTEXT((#26958))
GLOBAL_UNIT_ASSIGNED_CONTEXT((#27070,#27072,#27073))
REPRESENTATION_CONTEXT('','3D')
);
#27036=(
GEOMETRIC_REPRESENTATION_CONTEXT(3)
GLOBAL_UNCERTAINTY_ASSIGNED_CONTEXT((#26959))
GLOBAL_UNIT_ASSIGNED_CONTEXT((#27070,#27072,#27073))
REPRESENTATION_CONTEXT('','3D')
);
#27037=(
GEOMETRIC_REPRESENTATION_CONTEXT(3)
GLOBAL_UNCERTAINTY_ASSIGNED_CONTEXT((#26960))
GLOBAL_UNIT_ASSIGNED_CONTEXT((#27070,#27072,#27073))
REPRESENTATION_CONTEXT('','3D')
);
#27038=(
GEOMETRIC_REPRESENTATION_CONTEXT(3)
GLOBAL_UNCERTAINTY_ASSIGNED_CONTEXT((#26961))
GLOBAL_UNIT_ASSIGNED_CONTEXT((#27070,#27072,#27073))
REPRESENTATION_CONTEXT('','3D')
);
#27039=(
GEOMETRIC_REPRESENTATION_CONTEXT(3)
GLOBAL_UNCERTAINTY_ASSIGNED_CONTEXT((#26962))
GLOBAL_UNIT_ASSIGNED_CONTEXT((#27070,#27072,#27073))
REPRESENTATION_CONTEXT('','3D')
);
#27040=(
GEOMETRIC_REPRESENTATION_CONTEXT(3)
GLOBAL_UNCERTAINTY_ASSIGNED_CONTEXT((#26963))
GLOBAL_UNIT_ASSIGNED_CONTEXT((#27070,#27072,#27073))
REPRESENTATION_CONTEXT('','3D')
);
#27041=(
GEOMETRIC_REPRESENTATION_CONTEXT(3)
GLOBAL_UNCERTAINTY_ASSIGNED_CONTEXT((#26964))
GLOBAL_UNIT_ASSIGNED_CONTEXT((#27070,#27072,#27073))
REPRESENTATION_CONTEXT('','3D')
);
#27042=(
GEOMETRIC_REPRESENTATION_CONTEXT(3)
GLOBAL_UNCERTAINTY_ASSIGNED_CONTEXT((#26965))
GLOBAL_UNIT_ASSIGNED_CONTEXT((#27070,#27072,#27073))
REPRESENTATION_CONTEXT('','3D')
);
#27043=(
GEOMETRIC_REPRESENTATION_CONTEXT(3)
GLOBAL_UNCERTAINTY_ASSIGNED_CONTEXT((#26966))
GLOBAL_UNIT_ASSIGNED_CONTEXT((#27070,#27072,#27073))
REPRESENTATION_CONTEXT('','3D')
);
#27044=(
GEOMETRIC_REPRESENTATION_CONTEXT(3)
GLOBAL_UNCERTAINTY_ASSIGNED_CONTEXT((#26967))
GLOBAL_UNIT_ASSIGNED_CONTEXT((#27070,#27072,#27073))
REPRESENTATION_CONTEXT('','3D')
);
#27045=(
GEOMETRIC_REPRESENTATION_CONTEXT(3)
GLOBAL_UNCERTAINTY_ASSIGNED_CONTEXT((#26968))
GLOBAL_UNIT_ASSIGNED_CONTEXT((#27070,#27072,#27073))
REPRESENTATION_CONTEXT('','3D')
);
#27046=(
GEOMETRIC_REPRESENTATION_CONTEXT(3)
GLOBAL_UNCERTAINTY_ASSIGNED_CONTEXT((#26969))
GLOBAL_UNIT_ASSIGNED_CONTEXT((#27070,#27072,#27073))
REPRESENTATION_CONTEXT('','3D')
);
#27047=(
GEOMETRIC_REPRESENTATION_CONTEXT(3)
GLOBAL_UNCERTAINTY_ASSIGNED_CONTEXT((#26970))
GLOBAL_UNIT_ASSIGNED_CONTEXT((#27070,#27072,#27073))
REPRESENTATION_CONTEXT('','3D')
);
#27048=(
GEOMETRIC_REPRESENTATION_CONTEXT(3)
GLOBAL_UNCERTAINTY_ASSIGNED_CONTEXT((#26971))
GLOBAL_UNIT_ASSIGNED_CONTEXT((#27070,#27072,#27073))
REPRESENTATION_CONTEXT('','3D')
);
#27049=(
GEOMETRIC_REPRESENTATION_CONTEXT(3)
GLOBAL_UNCERTAINTY_ASSIGNED_CONTEXT((#26972))
GLOBAL_UNIT_ASSIGNED_CONTEXT((#27070,#27072,#27073))
REPRESENTATION_CONTEXT('','3D')
);
#27050=(
GEOMETRIC_REPRESENTATION_CONTEXT(3)
GLOBAL_UNCERTAINTY_ASSIGNED_CONTEXT((#26973))
GLOBAL_UNIT_ASSIGNED_CONTEXT((#27070,#27072,#27073))
REPRESENTATION_CONTEXT('','3D')
);
#27051=(
GEOMETRIC_REPRESENTATION_CONTEXT(3)
GLOBAL_UNCERTAINTY_ASSIGNED_CONTEXT((#26974))
GLOBAL_UNIT_ASSIGNED_CONTEXT((#27070,#27072,#27073))
REPRESENTATION_CONTEXT('','3D')
);
#27052=(
GEOMETRIC_REPRESENTATION_CONTEXT(3)
GLOBAL_UNCERTAINTY_ASSIGNED_CONTEXT((#26975))
GLOBAL_UNIT_ASSIGNED_CONTEXT((#27070,#27072,#27073))
REPRESENTATION_CONTEXT('','3D')
);
#27053=(
GEOMETRIC_REPRESENTATION_CONTEXT(3)
GLOBAL_UNCERTAINTY_ASSIGNED_CONTEXT((#26976))
GLOBAL_UNIT_ASSIGNED_CONTEXT((#27070,#27072,#27073))
REPRESENTATION_CONTEXT('','3D')
);
#27054=(
GEOMETRIC_REPRESENTATION_CONTEXT(3)
GLOBAL_UNCERTAINTY_ASSIGNED_CONTEXT((#26977))
GLOBAL_UNIT_ASSIGNED_CONTEXT((#27070,#27072,#27073))
REPRESENTATION_CONTEXT('','3D')
);
#27055=(
GEOMETRIC_REPRESENTATION_CONTEXT(3)
GLOBAL_UNCERTAINTY_ASSIGNED_CONTEXT((#26978))
GLOBAL_UNIT_ASSIGNED_CONTEXT((#27070,#27072,#27073))
REPRESENTATION_CONTEXT('','3D')
);
#27056=(
GEOMETRIC_REPRESENTATION_CONTEXT(3)
GLOBAL_UNCERTAINTY_ASSIGNED_CONTEXT((#26979))
GLOBAL_UNIT_ASSIGNED_CONTEXT((#27070,#27072,#27073))
REPRESENTATION_CONTEXT('','3D')
);
#27057=(
GEOMETRIC_REPRESENTATION_CONTEXT(3)
GLOBAL_UNCERTAINTY_ASSIGNED_CONTEXT((#26980))
GLOBAL_UNIT_ASSIGNED_CONTEXT((#27070,#27072,#27073))
REPRESENTATION_CONTEXT('','3D')
);
#27058=(
GEOMETRIC_REPRESENTATION_CONTEXT(3)
GLOBAL_UNCERTAINTY_ASSIGNED_CONTEXT((#26981))
GLOBAL_UNIT_ASSIGNED_CONTEXT((#27070,#27072,#27073))
REPRESENTATION_CONTEXT('','3D')
);
#27059=(
GEOMETRIC_REPRESENTATION_CONTEXT(3)
GLOBAL_UNCERTAINTY_ASSIGNED_CONTEXT((#26982))
GLOBAL_UNIT_ASSIGNED_CONTEXT((#27070,#27072,#27073))
REPRESENTATION_CONTEXT('','3D')
);
#27060=(
GEOMETRIC_REPRESENTATION_CONTEXT(3)
GLOBAL_UNCERTAINTY_ASSIGNED_CONTEXT((#26983))
GLOBAL_UNIT_ASSIGNED_CONTEXT((#27070,#27072,#27073))
REPRESENTATION_CONTEXT('','3D')
);
#27061=(
GEOMETRIC_REPRESENTATION_CONTEXT(3)
GLOBAL_UNCERTAINTY_ASSIGNED_CONTEXT((#26984))
GLOBAL_UNIT_ASSIGNED_CONTEXT((#27070,#27072,#27073))
REPRESENTATION_CONTEXT('','3D')
);
#27062=(
GEOMETRIC_REPRESENTATION_CONTEXT(3)
GLOBAL_UNCERTAINTY_ASSIGNED_CONTEXT((#26985))
GLOBAL_UNIT_ASSIGNED_CONTEXT((#27070,#27072,#27073))
REPRESENTATION_CONTEXT('','3D')
);
#27063=(
GEOMETRIC_REPRESENTATION_CONTEXT(3)
GLOBAL_UNCERTAINTY_ASSIGNED_CONTEXT((#26986))
GLOBAL_UNIT_ASSIGNED_CONTEXT((#27070,#27072,#27073))
REPRESENTATION_CONTEXT('','3D')
);
#27064=(
GEOMETRIC_REPRESENTATION_CONTEXT(3)
GLOBAL_UNCERTAINTY_ASSIGNED_CONTEXT((#26987))
GLOBAL_UNIT_ASSIGNED_CONTEXT((#27070,#27072,#27073))
REPRESENTATION_CONTEXT('','3D')
);
#27065=(
GEOMETRIC_REPRESENTATION_CONTEXT(3)
GLOBAL_UNCERTAINTY_ASSIGNED_CONTEXT((#26988))
GLOBAL_UNIT_ASSIGNED_CONTEXT((#27070,#27072,#27073))
REPRESENTATION_CONTEXT('','3D')
);
#27066=(
GEOMETRIC_REPRESENTATION_CONTEXT(3)
GLOBAL_UNCERTAINTY_ASSIGNED_CONTEXT((#26989))
GLOBAL_UNIT_ASSIGNED_CONTEXT((#27070,#27072,#27073))
REPRESENTATION_CONTEXT('','3D')
);
#27067=(
GEOMETRIC_REPRESENTATION_CONTEXT(3)
GLOBAL_UNCERTAINTY_ASSIGNED_CONTEXT((#26990))
GLOBAL_UNIT_ASSIGNED_CONTEXT((#27070,#27072,#27073))
REPRESENTATION_CONTEXT('','3D')
);
#27068=(
GEOMETRIC_REPRESENTATION_CONTEXT(3)
GLOBAL_UNCERTAINTY_ASSIGNED_CONTEXT((#26991))
GLOBAL_UNIT_ASSIGNED_CONTEXT((#27070,#27072,#27073))
REPRESENTATION_CONTEXT('','3D')
);
#27069=(
GEOMETRIC_REPRESENTATION_CONTEXT(3)
GLOBAL_UNCERTAINTY_ASSIGNED_CONTEXT((#26992))
GLOBAL_UNIT_ASSIGNED_CONTEXT((#27070,#27072,#27073))
REPRESENTATION_CONTEXT('','3D')
);
#27070=(
LENGTH_UNIT()
NAMED_UNIT(*)
SI_UNIT(.CENTI.,.METRE.)
);
#27071=(
LENGTH_UNIT()
NAMED_UNIT(*)
SI_UNIT($,.METRE.)
);
#27072=(
NAMED_UNIT(*)
PLANE_ANGLE_UNIT()
SI_UNIT($,.RADIAN.)
);
#27073=(
NAMED_UNIT(*)
SI_UNIT($,.STERADIAN.)
SOLID_ANGLE_UNIT()
);
#27074=SHAPE_DEFINITION_REPRESENTATION(#27150,#27351);
#27075=SHAPE_DEFINITION_REPRESENTATION(#27151,#27352);
#27076=SHAPE_DEFINITION_REPRESENTATION(#27152,#27353);
#27077=SHAPE_DEFINITION_REPRESENTATION(#27153,#27354);
#27078=SHAPE_DEFINITION_REPRESENTATION(#27154,#27355);
#27079=SHAPE_DEFINITION_REPRESENTATION(#27155,#27356);
#27080=SHAPE_DEFINITION_REPRESENTATION(#27156,#27357);
#27081=SHAPE_DEFINITION_REPRESENTATION(#27157,#27358);
#27082=SHAPE_DEFINITION_REPRESENTATION(#27158,#27359);
#27083=SHAPE_DEFINITION_REPRESENTATION(#27159,#27360);
#27084=SHAPE_DEFINITION_REPRESENTATION(#27160,#27361);
#27085=SHAPE_DEFINITION_REPRESENTATION(#27161,#27362);
#27086=SHAPE_DEFINITION_REPRESENTATION(#27162,#27363);
#27087=SHAPE_DEFINITION_REPRESENTATION(#27163,#27364);
#27088=SHAPE_DEFINITION_REPRESENTATION(#27164,#27365);
#27089=SHAPE_DEFINITION_REPRESENTATION(#27165,#27366);
#27090=SHAPE_DEFINITION_REPRESENTATION(#27166,#27367);
#27091=SHAPE_DEFINITION_REPRESENTATION(#27167,#27368);
#27092=SHAPE_DEFINITION_REPRESENTATION(#27168,#27369);
#27093=SHAPE_DEFINITION_REPRESENTATION(#27169,#27370);
#27094=SHAPE_DEFINITION_REPRESENTATION(#27170,#27371);
#27095=SHAPE_DEFINITION_REPRESENTATION(#27171,#27372);
#27096=SHAPE_DEFINITION_REPRESENTATION(#27172,#27373);
#27097=SHAPE_DEFINITION_REPRESENTATION(#27173,#27374);
#27098=SHAPE_DEFINITION_REPRESENTATION(#27174,#27375);
#27099=SHAPE_DEFINITION_REPRESENTATION(#27175,#27376);
#27100=SHAPE_DEFINITION_REPRESENTATION(#27176,#27377);
#27101=SHAPE_DEFINITION_REPRESENTATION(#27177,#27378);
#27102=SHAPE_DEFINITION_REPRESENTATION(#27178,#27379);
#27103=SHAPE_DEFINITION_REPRESENTATION(#27179,#27380);
#27104=SHAPE_DEFINITION_REPRESENTATION(#27180,#27381);
#27105=SHAPE_DEFINITION_REPRESENTATION(#27181,#27382);
#27106=SHAPE_DEFINITION_REPRESENTATION(#27182,#27383);
#27107=SHAPE_DEFINITION_REPRESENTATION(#27183,#27384);
#27108=SHAPE_DEFINITION_REPRESENTATION(#27184,#27385);
#27109=SHAPE_DEFINITION_REPRESENTATION(#27190,#27386);
#27110=SHAPE_DEFINITION_REPRESENTATION(#27191,#27387);
#27111=SHAPE_DEFINITION_REPRESENTATION(#27192,#27388);
#27112=SHAPE_DEFINITION_REPRESENTATION(#27193,#27389);
#27113=SHAPE_DEFINITION_REPRESENTATION(#27194,#27390);
#27114=SHAPE_DEFINITION_REPRESENTATION(#27195,#27391);
#27115=SHAPE_DEFINITION_REPRESENTATION(#27196,#27392);
#27116=SHAPE_DEFINITION_REPRESENTATION(#27202,#27393);
#27117=SHAPE_DEFINITION_REPRESENTATION(#27203,#27394);
#27118=SHAPE_DEFINITION_REPRESENTATION(#27204,#27395);
#27119=SHAPE_DEFINITION_REPRESENTATION(#27205,#27396);
#27120=SHAPE_DEFINITION_REPRESENTATION(#27208,#27397);
#27121=SHAPE_DEFINITION_REPRESENTATION(#27209,#27398);
#27122=SHAPE_DEFINITION_REPRESENTATION(#27210,#27399);
#27123=SHAPE_DEFINITION_REPRESENTATION(#27211,#27400);
#27124=SHAPE_DEFINITION_REPRESENTATION(#27212,#27401);
#27125=SHAPE_DEFINITION_REPRESENTATION(#27213,#27402);
#27126=SHAPE_DEFINITION_REPRESENTATION(#27214,#27403);
#27127=SHAPE_DEFINITION_REPRESENTATION(#27215,#27404);
#27128=SHAPE_DEFINITION_REPRESENTATION(#27216,#27405);
#27129=SHAPE_DEFINITION_REPRESENTATION(#27217,#27406);
#27130=SHAPE_DEFINITION_REPRESENTATION(#27218,#27407);
#27131=SHAPE_DEFINITION_REPRESENTATION(#27219,#27408);
#27132=SHAPE_DEFINITION_REPRESENTATION(#27220,#27409);
#27133=SHAPE_DEFINITION_REPRESENTATION(#27221,#27410);
#27134=SHAPE_DEFINITION_REPRESENTATION(#27222,#27411);
#27135=SHAPE_DEFINITION_REPRESENTATION(#27223,#27412);
#27136=SHAPE_DEFINITION_REPRESENTATION(#27224,#27413);
#27137=SHAPE_DEFINITION_REPRESENTATION(#27225,#27414);
#27138=SHAPE_DEFINITION_REPRESENTATION(#27226,#27415);
#27139=SHAPE_DEFINITION_REPRESENTATION(#27227,#27416);
#27140=SHAPE_DEFINITION_REPRESENTATION(#27228,#27417);
#27141=SHAPE_DEFINITION_REPRESENTATION(#27229,#27418);
#27142=SHAPE_DEFINITION_REPRESENTATION(#27230,#27419);
#27143=SHAPE_DEFINITION_REPRESENTATION(#27231,#27420);
#27144=SHAPE_DEFINITION_REPRESENTATION(#27232,#27421);
#27145=SHAPE_DEFINITION_REPRESENTATION(#27233,#27422);
#27146=SHAPE_DEFINITION_REPRESENTATION(#27234,#27423);
#27147=SHAPE_DEFINITION_REPRESENTATION(#27235,#27424);
#27148=SHAPE_DEFINITION_REPRESENTATION(#27236,#27425);
#27149=SHAPE_DEFINITION_REPRESENTATION(#27316,#27426);
#27150=PRODUCT_DEFINITION_SHAPE('',$,#27428);
#27151=PRODUCT_DEFINITION_SHAPE('',$,#27429);
#27152=PRODUCT_DEFINITION_SHAPE('',$,#27430);
#27153=PRODUCT_DEFINITION_SHAPE('',$,#27431);
#27154=PRODUCT_DEFINITION_SHAPE('',$,#27432);
#27155=PRODUCT_DEFINITION_SHAPE('',$,#27433);
#27156=PRODUCT_DEFINITION_SHAPE('',$,#27434);
#27157=PRODUCT_DEFINITION_SHAPE('',$,#27435);
#27158=PRODUCT_DEFINITION_SHAPE('',$,#27436);
#27159=PRODUCT_DEFINITION_SHAPE('',$,#27437);
#27160=PRODUCT_DEFINITION_SHAPE('',$,#27438);
#27161=PRODUCT_DEFINITION_SHAPE('',$,#27439);
#27162=PRODUCT_DEFINITION_SHAPE('',$,#27440);
#27163=PRODUCT_DEFINITION_SHAPE('',$,#27441);
#27164=PRODUCT_DEFINITION_SHAPE('',$,#27442);
#27165=PRODUCT_DEFINITION_SHAPE('',$,#27443);
#27166=PRODUCT_DEFINITION_SHAPE('',$,#27444);
#27167=PRODUCT_DEFINITION_SHAPE('',$,#27445);
#27168=PRODUCT_DEFINITION_SHAPE('',$,#27446);
#27169=PRODUCT_DEFINITION_SHAPE('',$,#27447);
#27170=PRODUCT_DEFINITION_SHAPE('',$,#27448);
#27171=PRODUCT_DEFINITION_SHAPE('',$,#27449);
#27172=PRODUCT_DEFINITION_SHAPE('',$,#27450);
#27173=PRODUCT_DEFINITION_SHAPE('',$,#27451);
#27174=PRODUCT_DEFINITION_SHAPE('',$,#27452);
#27175=PRODUCT_DEFINITION_SHAPE('',$,#27453);
#27176=PRODUCT_DEFINITION_SHAPE('',$,#27454);
#27177=PRODUCT_DEFINITION_SHAPE('',$,#27455);
#27178=PRODUCT_DEFINITION_SHAPE('',$,#27456);
#27179=PRODUCT_DEFINITION_SHAPE('',$,#27457);
#27180=PRODUCT_DEFINITION_SHAPE('',$,#27458);
#27181=PRODUCT_DEFINITION_SHAPE('',$,#27459);
#27182=PRODUCT_DEFINITION_SHAPE('',$,#27460);
#27183=PRODUCT_DEFINITION_SHAPE('',$,#27461);
#27184=PRODUCT_DEFINITION_SHAPE('',$,#27462);
#27185=PRODUCT_DEFINITION_SHAPE($,$,#396);
#27186=PRODUCT_DEFINITION_SHAPE($,$,#397);
#27187=PRODUCT_DEFINITION_SHAPE($,$,#398);
#27188=PRODUCT_DEFINITION_SHAPE($,$,#399);
#27189=PRODUCT_DEFINITION_SHAPE($,$,#400);
#27190=PRODUCT_DEFINITION_SHAPE('',$,#27463);
#27191=PRODUCT_DEFINITION_SHAPE('',$,#27464);
#27192=PRODUCT_DEFINITION_SHAPE('',$,#27465);
#27193=PRODUCT_DEFINITION_SHAPE('',$,#27466);
#27194=PRODUCT_DEFINITION_SHAPE('',$,#27467);
#27195=PRODUCT_DEFINITION_SHAPE('',$,#27468);
#27196=PRODUCT_DEFINITION_SHAPE('',$,#27469);
#27197=PRODUCT_DEFINITION_SHAPE($,$,#401);
#27198=PRODUCT_DEFINITION_SHAPE($,$,#402);
#27199=PRODUCT_DEFINITION_SHAPE($,$,#403);
#27200=PRODUCT_DEFINITION_SHAPE($,$,#404);
#27201=PRODUCT_DEFINITION_SHAPE($,$,#405);
#27202=PRODUCT_DEFINITION_SHAPE('',$,#27470);
#27203=PRODUCT_DEFINITION_SHAPE('',$,#27471);
#27204=PRODUCT_DEFINITION_SHAPE('',$,#27472);
#27205=PRODUCT_DEFINITION_SHAPE('',$,#27473);
#27206=PRODUCT_DEFINITION_SHAPE($,$,#406);
#27207=PRODUCT_DEFINITION_SHAPE($,$,#407);
#27208=PRODUCT_DEFINITION_SHAPE('',$,#27474);
#27209=PRODUCT_DEFINITION_SHAPE('',$,#27475);
#27210=PRODUCT_DEFINITION_SHAPE('',$,#27476);
#27211=PRODUCT_DEFINITION_SHAPE('',$,#27477);
#27212=PRODUCT_DEFINITION_SHAPE('',$,#27478);
#27213=PRODUCT_DEFINITION_SHAPE('',$,#27479);
#27214=PRODUCT_DEFINITION_SHAPE('',$,#27480);
#27215=PRODUCT_DEFINITION_SHAPE('',$,#27481);
#27216=PRODUCT_DEFINITION_SHAPE('',$,#27482);
#27217=PRODUCT_DEFINITION_SHAPE('',$,#27483);
#27218=PRODUCT_DEFINITION_SHAPE('',$,#27484);
#27219=PRODUCT_DEFINITION_SHAPE('',$,#27485);
#27220=PRODUCT_DEFINITION_SHAPE('',$,#27486);
#27221=PRODUCT_DEFINITION_SHAPE('',$,#27487);
#27222=PRODUCT_DEFINITION_SHAPE('',$,#27488);
#27223=PRODUCT_DEFINITION_SHAPE('',$,#27489);
#27224=PRODUCT_DEFINITION_SHAPE('',$,#27490);
#27225=PRODUCT_DEFINITION_SHAPE('',$,#27491);
#27226=PRODUCT_DEFINITION_SHAPE('',$,#27492);
#27227=PRODUCT_DEFINITION_SHAPE('',$,#27493);
#27228=PRODUCT_DEFINITION_SHAPE('',$,#27494);
#27229=PRODUCT_DEFINITION_SHAPE('',$,#27495);
#27230=PRODUCT_DEFINITION_SHAPE('',$,#27496);
#27231=PRODUCT_DEFINITION_SHAPE('',$,#27497);
#27232=PRODUCT_DEFINITION_SHAPE('',$,#27498);
#27233=PRODUCT_DEFINITION_SHAPE('',$,#27499);
#27234=PRODUCT_DEFINITION_SHAPE('',$,#27500);
#27235=PRODUCT_DEFINITION_SHAPE('',$,#27501);
#27236=PRODUCT_DEFINITION_SHAPE('',$,#27502);
#27237=PRODUCT_DEFINITION_SHAPE($,$,#408);
#27238=PRODUCT_DEFINITION_SHAPE($,$,#409);
#27239=PRODUCT_DEFINITION_SHAPE($,$,#410);
#27240=PRODUCT_DEFINITION_SHAPE($,$,#411);
#27241=PRODUCT_DEFINITION_SHAPE($,$,#412);
#27242=PRODUCT_DEFINITION_SHAPE($,$,#413);
#27243=PRODUCT_DEFINITION_SHAPE($,$,#414);
#27244=PRODUCT_DEFINITION_SHAPE($,$,#415);
#27245=PRODUCT_DEFINITION_SHAPE($,$,#416);
#27246=PRODUCT_DEFINITION_SHAPE($,$,#417);
#27247=PRODUCT_DEFINITION_SHAPE($,$,#418);
#27248=PRODUCT_DEFINITION_SHAPE($,$,#419);
#27249=PRODUCT_DEFINITION_SHAPE($,$,#420);
#27250=PRODUCT_DEFINITION_SHAPE($,$,#421);
#27251=PRODUCT_DEFINITION_SHAPE($,$,#422);
#27252=PRODUCT_DEFINITION_SHAPE($,$,#423);
#27253=PRODUCT_DEFINITION_SHAPE($,$,#424);
#27254=PRODUCT_DEFINITION_SHAPE($,$,#425);
#27255=PRODUCT_DEFINITION_SHAPE($,$,#426);
#27256=PRODUCT_DEFINITION_SHAPE($,$,#427);
#27257=PRODUCT_DEFINITION_SHAPE($,$,#428);
#27258=PRODUCT_DEFINITION_SHAPE($,$,#429);
#27259=PRODUCT_DEFINITION_SHAPE($,$,#430);
#27260=PRODUCT_DEFINITION_SHAPE($,$,#431);
#27261=PRODUCT_DEFINITION_SHAPE($,$,#432);
#27262=PRODUCT_DEFINITION_SHAPE($,$,#433);
#27263=PRODUCT_DEFINITION_SHAPE($,$,#434);
#27264=PRODUCT_DEFINITION_SHAPE($,$,#435);
#27265=PRODUCT_DEFINITION_SHAPE($,$,#436);
#27266=PRODUCT_DEFINITION_SHAPE($,$,#437);
#27267=PRODUCT_DEFINITION_SHAPE($,$,#438);
#27268=PRODUCT_DEFINITION_SHAPE($,$,#439);
#27269=PRODUCT_DEFINITION_SHAPE($,$,#440);
#27270=PRODUCT_DEFINITION_SHAPE($,$,#441);
#27271=PRODUCT_DEFINITION_SHAPE($,$,#442);
#27272=PRODUCT_DEFINITION_SHAPE($,$,#443);
#27273=PRODUCT_DEFINITION_SHAPE($,$,#444);
#27274=PRODUCT_DEFINITION_SHAPE($,$,#445);
#27275=PRODUCT_DEFINITION_SHAPE($,$,#446);
#27276=PRODUCT_DEFINITION_SHAPE($,$,#447);
#27277=PRODUCT_DEFINITION_SHAPE($,$,#448);
#27278=PRODUCT_DEFINITION_SHAPE($,$,#449);
#27279=PRODUCT_DEFINITION_SHAPE($,$,#450);
#27280=PRODUCT_DEFINITION_SHAPE($,$,#451);
#27281=PRODUCT_DEFINITION_SHAPE($,$,#452);
#27282=PRODUCT_DEFINITION_SHAPE($,$,#453);
#27283=PRODUCT_DEFINITION_SHAPE($,$,#454);
#27284=PRODUCT_DEFINITION_SHAPE($,$,#455);
#27285=PRODUCT_DEFINITION_SHAPE($,$,#456);
#27286=PRODUCT_DEFINITION_SHAPE($,$,#457);
#27287=PRODUCT_DEFINITION_SHAPE($,$,#458);
#27288=PRODUCT_DEFINITION_SHAPE($,$,#459);
#27289=PRODUCT_DEFINITION_SHAPE($,$,#460);
#27290=PRODUCT_DEFINITION_SHAPE($,$,#461);
#27291=PRODUCT_DEFINITION_SHAPE($,$,#462);
#27292=PRODUCT_DEFINITION_SHAPE($,$,#463);
#27293=PRODUCT_DEFINITION_SHAPE($,$,#464);
#27294=PRODUCT_DEFINITION_SHAPE($,$,#465);
#27295=PRODUCT_DEFINITION_SHAPE($,$,#466);
#27296=PRODUCT_DEFINITION_SHAPE($,$,#467);
#27297=PRODUCT_DEFINITION_SHAPE($,$,#468);
#27298=PRODUCT_DEFINITION_SHAPE($,$,#469);
#27299=PRODUCT_DEFINITION_SHAPE($,$,#470);
#27300=PRODUCT_DEFINITION_SHAPE($,$,#471);
#27301=PRODUCT_DEFINITION_SHAPE($,$,#472);
#27302=PRODUCT_DEFINITION_SHAPE($,$,#473);
#27303=PRODUCT_DEFINITION_SHAPE($,$,#474);
#27304=PRODUCT_DEFINITION_SHAPE($,$,#475);
#27305=PRODUCT_DEFINITION_SHAPE($,$,#476);
#27306=PRODUCT_DEFINITION_SHAPE($,$,#477);
#27307=PRODUCT_DEFINITION_SHAPE($,$,#478);
#27308=PRODUCT_DEFINITION_SHAPE($,$,#479);
#27309=PRODUCT_DEFINITION_SHAPE($,$,#480);
#27310=PRODUCT_DEFINITION_SHAPE($,$,#481);
#27311=PRODUCT_DEFINITION_SHAPE($,$,#482);
#27312=PRODUCT_DEFINITION_SHAPE($,$,#483);
#27313=PRODUCT_DEFINITION_SHAPE($,$,#484);
#27314=PRODUCT_DEFINITION_SHAPE($,$,#485);
#27315=PRODUCT_DEFINITION_SHAPE($,$,#486);
#27316=PRODUCT_DEFINITION_SHAPE('',$,#27503);
#27317=PRODUCT_DEFINITION_SHAPE($,$,#487);
#27318=PRODUCT_DEFINITION_SHAPE($,$,#488);
#27319=PRODUCT_DEFINITION_SHAPE($,$,#489);
#27320=PRODUCT_DEFINITION_SHAPE($,$,#490);
#27321=PRODUCT_DEFINITION_SHAPE($,$,#491);
#27322=PRODUCT_DEFINITION_SHAPE($,$,#492);
#27323=PRODUCT_DEFINITION_SHAPE($,$,#493);
#27324=PRODUCT_DEFINITION_SHAPE($,$,#494);
#27325=PRODUCT_DEFINITION_SHAPE($,$,#495);
#27326=PRODUCT_DEFINITION_SHAPE($,$,#496);
#27327=PRODUCT_DEFINITION_SHAPE($,$,#497);
#27328=PRODUCT_DEFINITION_SHAPE($,$,#498);
#27329=PRODUCT_DEFINITION_SHAPE($,$,#499);
#27330=PRODUCT_DEFINITION_SHAPE($,$,#500);
#27331=PRODUCT_DEFINITION_SHAPE($,$,#501);
#27332=PRODUCT_DEFINITION_SHAPE($,$,#502);
#27333=PRODUCT_DEFINITION_SHAPE($,$,#503);
#27334=PRODUCT_DEFINITION_SHAPE($,$,#504);
#27335=PRODUCT_DEFINITION_SHAPE($,$,#505);
#27336=PRODUCT_DEFINITION_SHAPE($,$,#506);
#27337=PRODUCT_DEFINITION_SHAPE($,$,#507);
#27338=PRODUCT_DEFINITION_SHAPE($,$,#508);
#27339=PRODUCT_DEFINITION_SHAPE($,$,#509);
#27340=PRODUCT_DEFINITION_SHAPE($,$,#510);
#27341=PRODUCT_DEFINITION_SHAPE($,$,#511);
#27342=PRODUCT_DEFINITION_SHAPE($,$,#512);
#27343=PRODUCT_DEFINITION_SHAPE($,$,#513);
#27344=PRODUCT_DEFINITION_SHAPE($,$,#514);
#27345=PRODUCT_DEFINITION_SHAPE($,$,#515);
#27346=PRODUCT_DEFINITION_SHAPE($,$,#516);
#27347=PRODUCT_DEFINITION_SHAPE($,$,#517);
#27348=PRODUCT_DEFINITION_SHAPE($,$,#518);
#27349=PRODUCT_DEFINITION_SHAPE($,$,#519);
#27350=PRODUCT_DEFINITION_SHAPE($,$,#520);
#27351=SHAPE_REPRESENTATION('',(#14562,#16431,#16432,#16433),#26993);
#27352=SHAPE_REPRESENTATION('',(#14563,#16304,#16305,#16306,#16307,#16308,
#16309,#16310,#16311,#16312,#16313,#16314,#16315,#16316,#16317,#16318,#16319,
#16320,#16321,#16322,#16323,#16324,#16325,#16326,#16327,#16328,#16329,#16330,
#16331,#16332,#16333,#16334,#16335,#16336,#16337,#16338,#16339,#16340,#16341,
#16342,#16343,#16344,#16345,#16346,#16347,#16348,#16349,#16350,#16351,#16352,
#16353,#16354,#16355,#16356,#16357,#16358,#16359,#16360,#16361,#16362,#16363,
#16364,#16365,#16366,#16367,#16368,#16369,#16370,#16371,#16372,#16373,#16374,
#16375,#16376,#16377,#16378,#16379,#16380,#16381,#16382),#26994);
#27353=SHAPE_REPRESENTATION('',(#14564),#26995);
#27354=SHAPE_REPRESENTATION('',(#14663),#26996);
#27355=SHAPE_REPRESENTATION('',(#14670),#26997);
#27356=SHAPE_REPRESENTATION('',(#14677),#26998);
#27357=SHAPE_REPRESENTATION('',(#14715),#26999);
#27358=SHAPE_REPRESENTATION('',(#14724),#27000);
#27359=SHAPE_REPRESENTATION('',(#14758),#27001);
#27360=SHAPE_REPRESENTATION('',(#14792),#27002);
#27361=SHAPE_REPRESENTATION('',(#14842),#27003);
#27362=SHAPE_REPRESENTATION('',(#14851),#27004);
#27363=SHAPE_REPRESENTATION('',(#14860),#27005);
#27364=SHAPE_REPRESENTATION('',(#14869),#27006);
#27365=SHAPE_REPRESENTATION('',(#14878),#27007);
#27366=SHAPE_REPRESENTATION('',(#14887),#27008);
#27367=SHAPE_REPRESENTATION('',(#14921),#27009);
#27368=SHAPE_REPRESENTATION('',(#14975),#27010);
#27369=SHAPE_REPRESENTATION('',(#14994),#27011);
#27370=SHAPE_REPRESENTATION('',(#15037),#27012);
#27371=SHAPE_REPRESENTATION('',(#15046),#27013);
#27372=SHAPE_REPRESENTATION('',(#15055),#27014);
#27373=SHAPE_REPRESENTATION('',(#15098),#27015);
#27374=SHAPE_REPRESENTATION('',(#15107),#27016);
#27375=SHAPE_REPRESENTATION('',(#15116),#27017);
#27376=SHAPE_REPRESENTATION('',(#15137),#27018);
#27377=SHAPE_REPRESENTATION('',(#15144),#27019);
#27378=SHAPE_REPRESENTATION('',(#15157),#27020);
#27379=SHAPE_REPRESENTATION('',(#15170),#27021);
#27380=SHAPE_REPRESENTATION('',(#15189,#15318,#15319,#15320,#15321,#15322),
#27022);
#27381=SHAPE_REPRESENTATION('',(#15190),#27023);
#27382=SHAPE_REPRESENTATION('',(#15210),#27024);
#27383=SHAPE_REPRESENTATION('',(#15230),#27025);
#27384=SHAPE_REPRESENTATION('',(#15247),#27026);
#27385=SHAPE_REPRESENTATION('',(#15301),#27027);
#27386=SHAPE_REPRESENTATION('',(#15323),#27028);
#27387=SHAPE_REPRESENTATION('',(#15353,#15476,#15477,#15478,#15479,#15480),
#27029);
#27388=SHAPE_REPRESENTATION('',(#15354),#27030);
#27389=SHAPE_REPRESENTATION('',(#15374),#27031);
#27390=SHAPE_REPRESENTATION('',(#15394),#27032);
#27391=SHAPE_REPRESENTATION('',(#15409),#27033);
#27392=SHAPE_REPRESENTATION('',(#15459),#27034);
#27393=SHAPE_REPRESENTATION('',(#15481),#27035);
#27394=SHAPE_REPRESENTATION('',(#15507,#15577,#15578),#27036);
#27395=SHAPE_REPRESENTATION('',(#15508),#27037);
#27396=SHAPE_REPRESENTATION('',(#15549),#27038);
#27397=SHAPE_REPRESENTATION('',(#15579),#27039);
#27398=SHAPE_REPRESENTATION('',(#15588),#27040);
#27399=SHAPE_REPRESENTATION('',(#15612),#27041);
#27400=SHAPE_REPRESENTATION('',(#15636,#16400,#16401,#16402,#16403,#16404,
#16405,#16406,#16407,#16408,#16409,#16410,#16411),#27042);
#27401=SHAPE_REPRESENTATION('',(#15637),#27043);
#27402=SHAPE_REPRESENTATION('',(#15659),#27044);
#27403=SHAPE_REPRESENTATION('',(#15672),#27045);
#27404=SHAPE_REPRESENTATION('',(#15681),#27046);
#27405=SHAPE_REPRESENTATION('',(#15687),#27047);
#27406=SHAPE_REPRESENTATION('',(#15693),#27048);
#27407=SHAPE_REPRESENTATION('',(#15702),#27049);
#27408=SHAPE_REPRESENTATION('',(#15708),#27050);
#27409=SHAPE_REPRESENTATION('',(#15729),#27051);
#27410=SHAPE_REPRESENTATION('',(#15871,#16412,#16413,#16414,#16415,#16416,
#16417,#16418,#16419,#16420,#16421,#16422,#16423,#16424,#16425,#16426,#16427,
#16428,#16429,#16430),#27052);
#27411=SHAPE_REPRESENTATION('',(#15872),#27053);
#27412=SHAPE_REPRESENTATION('',(#15890),#27054);
#27413=SHAPE_REPRESENTATION('',(#15899),#27055);
#27414=SHAPE_REPRESENTATION('',(#15908),#27056);
#27415=SHAPE_REPRESENTATION('',(#15914),#27057);
#27416=SHAPE_REPRESENTATION('',(#15920),#27058);
#27417=SHAPE_REPRESENTATION('',(#15929),#27059);
#27418=SHAPE_REPRESENTATION('',(#15944),#27060);
#27419=SHAPE_REPRESENTATION('',(#15959),#27061);
#27420=SHAPE_REPRESENTATION('',(#15968),#27062);
#27421=SHAPE_REPRESENTATION('',(#15977),#27063);
#27422=SHAPE_REPRESENTATION('',(#15986),#27064);
#27423=SHAPE_REPRESENTATION('',(#16001),#27065);
#27424=SHAPE_REPRESENTATION('',(#16016),#27066);
#27425=SHAPE_REPRESENTATION('',(#16278),#27067);
#27426=SHAPE_REPRESENTATION('',(#16383),#27068);
#27427=PRODUCT_DEFINITION_CONTEXT('part definition',#27657,'design');
#27428=PRODUCT_DEFINITION('PAT-010','PAT-010',#27504,
#27427);
#27429=PRODUCT_DEFINITION('Bearing base and belt envelope',
'Bearing base and belt envelope',#27505,#27427);
#27430=PRODUCT_DEFINITION('Base','Base',#27506,#27427);
#27431=PRODUCT_DEFINITION('Foot','Foot',#27507,#27427);
#27432=PRODUCT_DEFINITION('Foot (1)','Foot (1)',#27508,#27427);
#27433=PRODUCT_DEFINITION('Fixed bearing block','Fixed bearing block',#27509,
#27427);
#27434=PRODUCT_DEFINITION('Input outer spacer','Input outer spacer',#27510,
#27427);
#27435=PRODUCT_DEFINITION('Input bearing cap','Input bearing cap',#27511,
#27427);
#27436=PRODUCT_DEFINITION('Input bearing cap (1)','Input bearing cap (1)',
#27512,#27427);
#27437=PRODUCT_DEFINITION('Sliding bearing block',
'Sliding bearing block',#27513,#27427);
#27438=PRODUCT_DEFINITION('M4 clamp nut','M4 clamp nut',#27514,#27427);
#27439=PRODUCT_DEFINITION('M4 clamp nut (1)','M4 clamp nut (1)',#27515,#27427);
#27440=PRODUCT_DEFINITION('M4 clamp nut (2)','M4 clamp nut (2)',#27516,#27427);
#27441=PRODUCT_DEFINITION('M4 clamp nut (3)','M4 clamp nut (3)',#27517,#27427);
#27442=PRODUCT_DEFINITION('Output outer spacer','Output outer spacer',#27518,
#27427);
#27443=PRODUCT_DEFINITION('Output bearing cap','Output bearing cap',#27519,
#27427);
#27444=PRODUCT_DEFINITION('Output bearing cap (1)',
'Output bearing cap (1)',#27520,#27427);
#27445=PRODUCT_DEFINITION('Timing belt backing envelope',
'Timing belt backing envelope',#27521,#27427);
#27446=PRODUCT_DEFINITION('Drum bearing riser','Drum bearing riser',#27522,
#27427);
#27447=PRODUCT_DEFINITION('Bearing mounting bush',
'Bearing mounting bush',#27523,#27427);
#27448=PRODUCT_DEFINITION('Bearing mounting bush (1)',
'Bearing mounting bush (1)',#27524,#27427);
#27449=PRODUCT_DEFINITION('Drum bearing riser (1)',
'Drum bearing riser (1)',#27525,#27427);
#27450=PRODUCT_DEFINITION('Bearing mounting bush (2)',
'Bearing mounting bush (2)',#27526,#27427);
#27451=PRODUCT_DEFINITION('Bearing mounting bush (3)',
'Bearing mounting bush (3)',#27527,#27427);
#27452=PRODUCT_DEFINITION('Motor pedestal','Motor pedestal',#27528,#27427);
#27453=PRODUCT_DEFINITION('Motor envelope','Motor envelope',#27529,#27427);
#27454=PRODUCT_DEFINITION('Guard post','Guard post',#27530,#27427);
#27455=PRODUCT_DEFINITION('Guard post (1)','Guard post (1)',#27531,#27427);
#27456=PRODUCT_DEFINITION('Belt guard','Belt guard',#27532,#27427);
#27457=PRODUCT_DEFINITION('Sealed Ball Bearing - 10 x 30 x 9 mm',
'Sealed Ball Bearing - 10 x 30 x 9 mm',#27533,#27427);
#27458=PRODUCT_DEFINITION('Inner ring','Inner ring',#27534,#27427);
#27459=PRODUCT_DEFINITION('Outer ring','Outer ring',#27535,#27427);
#27460=PRODUCT_DEFINITION('Balls','Balls',#27536,#27427);
#27461=PRODUCT_DEFINITION('Cage','Cage',#27537,#27427);
#27462=PRODUCT_DEFINITION('Seals 2RS','Seals 2RS',#27538,#27427);
#27463=PRODUCT_DEFINITION('M4x30 mounting screw','M4x30 mounting screw',
#27539,#27427);
#27464=PRODUCT_DEFINITION('Sealed Ball Bearing - 12 x 32 x 10 mm',
'Sealed Ball Bearing - 12 x 32 x 10 mm',#27540,#27427);
#27465=PRODUCT_DEFINITION('Inner ring (1)','Inner ring (1)',#27541,#27427);
#27466=PRODUCT_DEFINITION('Outer ring (1)','Outer ring (1)',#27542,#27427);
#27467=PRODUCT_DEFINITION('Balls (1)','Balls (1)',#27543,#27427);
#27468=PRODUCT_DEFINITION('Cage (1)','Cage (1)',#27544,#27427);
#27469=PRODUCT_DEFINITION('Seals 2RS (1)','Seals 2RS (1)',#27545,#27427);
#27470=PRODUCT_DEFINITION('Cap Screw - M5x20','Cap Screw - M5x20',#27546,
#27427);
#27471=PRODUCT_DEFINITION('Pillow Block Bearing - 20 mm Bore',
'Pillow Block Bearing - 20 mm Bore',#27547,#27427);
#27472=PRODUCT_DEFINITION('Housing','Housing',#27548,#27427);
#27473=PRODUCT_DEFINITION('Insert bearing','Insert bearing',#27549,#27427);
#27474=PRODUCT_DEFINITION('Flat Washer - M8','Flat Washer - M8',#27550,
#27427);
#27475=PRODUCT_DEFINITION('M8x25 Bolt','M8x25 Bolt',#27551,#27427);
#27476=PRODUCT_DEFINITION('M4x10 Cap Screw','M4x10 Cap Screw',#27552,#27427);
#27477=PRODUCT_DEFINITION('Input pulley and shaft',
'Input pulley and shaft',#27553,#27427);
#27478=PRODUCT_DEFINITION('Input shaft','Input shaft',#27554,#27427);
#27479=PRODUCT_DEFINITION('Input inner spacer','Input inner spacer',#27555,
#27427);
#27480=PRODUCT_DEFINITION('Input inner sleeve','Input inner sleeve',#27556,
#27427);
#27481=PRODUCT_DEFINITION('Input M3 set screw','Input M3 set screw',#27557,
#27427);
#27482=PRODUCT_DEFINITION('Input M3 set screw (1)',
'Input M3 set screw (1)',#27558,#27427);
#27483=PRODUCT_DEFINITION('Input end keeper','Input end keeper',#27559,
#27427);
#27484=PRODUCT_DEFINITION('Motor output shaft','Motor output shaft',#27560,
#27427);
#27485=PRODUCT_DEFINITION('Motor coupling','Motor coupling',#27561,#27427);
#27486=PRODUCT_DEFINITION(
'Timing Pulley - 2 mm Pitch, 20 Teeth, 8 mm Bore',
'Timing Pulley - 2 mm Pitch, 20 Teeth, 8 mm Bore',#27562,#27427);
#27487=PRODUCT_DEFINITION('Output pulley and shaft',
'Output pulley and shaft',#27563,#27427);
#27488=PRODUCT_DEFINITION('Output shaft','Output shaft',#27564,#27427);
#27489=PRODUCT_DEFINITION('Output inner spacer','Output inner spacer',#27565,
#27427);
#27490=PRODUCT_DEFINITION('Output inner sleeve','Output inner sleeve',#27566,
#27427);
#27491=PRODUCT_DEFINITION('Output M3 set screw','Output M3 set screw',#27567,
#27427);
#27492=PRODUCT_DEFINITION('Output M3 set screw (1)',
'Output M3 set screw (1)',#27568,#27427);
#27493=PRODUCT_DEFINITION('Output end keeper','Output end keeper',#27569,
#27427);
#27494=PRODUCT_DEFINITION('Drum shaft collar','Drum shaft collar',#27570,
#27427);
#27495=PRODUCT_DEFINITION('Drum shaft collar (1)','Drum shaft collar (1)',
#27571,#27427);
#27496=PRODUCT_DEFINITION('Conveyor drum shell','Conveyor drum shell',#27572,
#27427);
#27497=PRODUCT_DEFINITION('Drum end plate','Drum end plate',#27573,#27427);
#27498=PRODUCT_DEFINITION('Drum end plate (1)','Drum end plate (1)',#27574,
#27427);
#27499=PRODUCT_DEFINITION('Drum hub','Drum hub',#27575,#27427);
#27500=PRODUCT_DEFINITION('Drum hub (1)','Drum hub (1)',#27576,#27427);
#27501=PRODUCT_DEFINITION(
'Timing Pulley - 2 mm Pitch, 40 Teeth, 12 mm Bore',
'Timing Pulley - 2 mm Pitch, 40 Teeth, 12 mm Bore',#27577,#27427);
#27502=PRODUCT_DEFINITION('Cap Screw - M4x16','Cap Screw - M4x16',#27578,
#27427);
#27503=PRODUCT_DEFINITION('Socket Set Screw - M5x8',
'Socket Set Screw - M5x8',#27579,#27427);
#27504=PRODUCT_DEFINITION_FORMATION('',$,#27659);
#27505=PRODUCT_DEFINITION_FORMATION('',$,#27660);
#27506=PRODUCT_DEFINITION_FORMATION('',$,#27661);
#27507=PRODUCT_DEFINITION_FORMATION('',$,#27662);
#27508=PRODUCT_DEFINITION_FORMATION('',$,#27663);
#27509=PRODUCT_DEFINITION_FORMATION('',$,#27664);
#27510=PRODUCT_DEFINITION_FORMATION('',$,#27665);
#27511=PRODUCT_DEFINITION_FORMATION('',$,#27666);
#27512=PRODUCT_DEFINITION_FORMATION('',$,#27667);
#27513=PRODUCT_DEFINITION_FORMATION('',$,#27668);
#27514=PRODUCT_DEFINITION_FORMATION('',$,#27669);
#27515=PRODUCT_DEFINITION_FORMATION('',$,#27670);
#27516=PRODUCT_DEFINITION_FORMATION('',$,#27671);
#27517=PRODUCT_DEFINITION_FORMATION('',$,#27672);
#27518=PRODUCT_DEFINITION_FORMATION('',$,#27673);
#27519=PRODUCT_DEFINITION_FORMATION('',$,#27674);
#27520=PRODUCT_DEFINITION_FORMATION('',$,#27675);
#27521=PRODUCT_DEFINITION_FORMATION('',$,#27676);
#27522=PRODUCT_DEFINITION_FORMATION('',$,#27677);
#27523=PRODUCT_DEFINITION_FORMATION('',$,#27678);
#27524=PRODUCT_DEFINITION_FORMATION('',$,#27679);
#27525=PRODUCT_DEFINITION_FORMATION('',$,#27680);
#27526=PRODUCT_DEFINITION_FORMATION('',$,#27681);
#27527=PRODUCT_DEFINITION_FORMATION('',$,#27682);
#27528=PRODUCT_DEFINITION_FORMATION('',$,#27683);
#27529=PRODUCT_DEFINITION_FORMATION('',$,#27684);
#27530=PRODUCT_DEFINITION_FORMATION('',$,#27685);
#27531=PRODUCT_DEFINITION_FORMATION('',$,#27686);
#27532=PRODUCT_DEFINITION_FORMATION('',$,#27687);
#27533=PRODUCT_DEFINITION_FORMATION('',$,#27688);
#27534=PRODUCT_DEFINITION_FORMATION('',$,#27689);
#27535=PRODUCT_DEFINITION_FORMATION('',$,#27690);
#27536=PRODUCT_DEFINITION_FORMATION('',$,#27691);
#27537=PRODUCT_DEFINITION_FORMATION('',$,#27692);
#27538=PRODUCT_DEFINITION_FORMATION('',$,#27693);
#27539=PRODUCT_DEFINITION_FORMATION('',$,#27694);
#27540=PRODUCT_DEFINITION_FORMATION('',$,#27695);
#27541=PRODUCT_DEFINITION_FORMATION('',$,#27696);
#27542=PRODUCT_DEFINITION_FORMATION('',$,#27697);
#27543=PRODUCT_DEFINITION_FORMATION('',$,#27698);
#27544=PRODUCT_DEFINITION_FORMATION('',$,#27699);
#27545=PRODUCT_DEFINITION_FORMATION('',$,#27700);
#27546=PRODUCT_DEFINITION_FORMATION('',$,#27701);
#27547=PRODUCT_DEFINITION_FORMATION('',$,#27702);
#27548=PRODUCT_DEFINITION_FORMATION('',$,#27703);
#27549=PRODUCT_DEFINITION_FORMATION('',$,#27704);
#27550=PRODUCT_DEFINITION_FORMATION('',$,#27705);
#27551=PRODUCT_DEFINITION_FORMATION('',$,#27706);
#27552=PRODUCT_DEFINITION_FORMATION('',$,#27707);
#27553=PRODUCT_DEFINITION_FORMATION('',$,#27708);
#27554=PRODUCT_DEFINITION_FORMATION('',$,#27709);
#27555=PRODUCT_DEFINITION_FORMATION('',$,#27710);
#27556=PRODUCT_DEFINITION_FORMATION('',$,#27711);
#27557=PRODUCT_DEFINITION_FORMATION('',$,#27712);
#27558=PRODUCT_DEFINITION_FORMATION('',$,#27713);
#27559=PRODUCT_DEFINITION_FORMATION('',$,#27714);
#27560=PRODUCT_DEFINITION_FORMATION('',$,#27715);
#27561=PRODUCT_DEFINITION_FORMATION('',$,#27716);
#27562=PRODUCT_DEFINITION_FORMATION('',$,#27717);
#27563=PRODUCT_DEFINITION_FORMATION('',$,#27718);
#27564=PRODUCT_DEFINITION_FORMATION('',$,#27719);
#27565=PRODUCT_DEFINITION_FORMATION('',$,#27720);
#27566=PRODUCT_DEFINITION_FORMATION('',$,#27721);
#27567=PRODUCT_DEFINITION_FORMATION('',$,#27722);
#27568=PRODUCT_DEFINITION_FORMATION('',$,#27723);
#27569=PRODUCT_DEFINITION_FORMATION('',$,#27724);
#27570=PRODUCT_DEFINITION_FORMATION('',$,#27725);
#27571=PRODUCT_DEFINITION_FORMATION('',$,#27726);
#27572=PRODUCT_DEFINITION_FORMATION('',$,#27727);
#27573=PRODUCT_DEFINITION_FORMATION('',$,#27728);
#27574=PRODUCT_DEFINITION_FORMATION('',$,#27729);
#27575=PRODUCT_DEFINITION_FORMATION('',$,#27730);
#27576=PRODUCT_DEFINITION_FORMATION('',$,#27731);
#27577=PRODUCT_DEFINITION_FORMATION('',$,#27732);
#27578=PRODUCT_DEFINITION_FORMATION('',$,#27733);
#27579=PRODUCT_DEFINITION_FORMATION('',$,#27734);
#27580=PRODUCT_RELATED_PRODUCT_CATEGORY('PAT-010','PAT-010',(#27659));
#27581=PRODUCT_RELATED_PRODUCT_CATEGORY(
'Bearing base and belt envelope','Bearing base and belt envelope',(#27660));
#27582=PRODUCT_RELATED_PRODUCT_CATEGORY('Base','Base',(#27661));
#27583=PRODUCT_RELATED_PRODUCT_CATEGORY('Foot','Foot',(#27662));
#27584=PRODUCT_RELATED_PRODUCT_CATEGORY('Foot (1)','Foot (1)',(#27663));
#27585=PRODUCT_RELATED_PRODUCT_CATEGORY('Fixed bearing block',
'Fixed bearing block',(#27664));
#27586=PRODUCT_RELATED_PRODUCT_CATEGORY('Input outer spacer',
'Input outer spacer',(#27665));
#27587=PRODUCT_RELATED_PRODUCT_CATEGORY('Input bearing cap',
'Input bearing cap',(#27666));
#27588=PRODUCT_RELATED_PRODUCT_CATEGORY('Input bearing cap (1)',
'Input bearing cap (1)',(#27667));
#27589=PRODUCT_RELATED_PRODUCT_CATEGORY('Sliding bearing block',
'Sliding bearing block',(#27668));
#27590=PRODUCT_RELATED_PRODUCT_CATEGORY('M4 clamp nut','M4 clamp nut',(#27669));
#27591=PRODUCT_RELATED_PRODUCT_CATEGORY('M4 clamp nut (1)',
'M4 clamp nut (1)',(#27670));
#27592=PRODUCT_RELATED_PRODUCT_CATEGORY('M4 clamp nut (2)',
'M4 clamp nut (2)',(#27671));
#27593=PRODUCT_RELATED_PRODUCT_CATEGORY('M4 clamp nut (3)',
'M4 clamp nut (3)',(#27672));
#27594=PRODUCT_RELATED_PRODUCT_CATEGORY('Output outer spacer',
'Output outer spacer',(#27673));
#27595=PRODUCT_RELATED_PRODUCT_CATEGORY('Output bearing cap',
'Output bearing cap',(#27674));
#27596=PRODUCT_RELATED_PRODUCT_CATEGORY('Output bearing cap (1)',
'Output bearing cap (1)',(#27675));
#27597=PRODUCT_RELATED_PRODUCT_CATEGORY('Timing belt backing envelope',
'Timing belt backing envelope',(#27676));
#27598=PRODUCT_RELATED_PRODUCT_CATEGORY('Drum bearing riser',
'Drum bearing riser',(#27677));
#27599=PRODUCT_RELATED_PRODUCT_CATEGORY('Bearing mounting bush',
'Bearing mounting bush',(#27678));
#27600=PRODUCT_RELATED_PRODUCT_CATEGORY('Bearing mounting bush (1)',
'Bearing mounting bush (1)',(#27679));
#27601=PRODUCT_RELATED_PRODUCT_CATEGORY('Drum bearing riser (1)',
'Drum bearing riser (1)',(#27680));
#27602=PRODUCT_RELATED_PRODUCT_CATEGORY('Bearing mounting bush (2)',
'Bearing mounting bush (2)',(#27681));
#27603=PRODUCT_RELATED_PRODUCT_CATEGORY('Bearing mounting bush (3)',
'Bearing mounting bush (3)',(#27682));
#27604=PRODUCT_RELATED_PRODUCT_CATEGORY('Motor pedestal',
'Motor pedestal',(#27683));
#27605=PRODUCT_RELATED_PRODUCT_CATEGORY('Motor envelope',
'Motor envelope',(#27684));
#27606=PRODUCT_RELATED_PRODUCT_CATEGORY('Guard post','Guard post',(#27685));
#27607=PRODUCT_RELATED_PRODUCT_CATEGORY('Guard post (1)',
'Guard post (1)',(#27686));
#27608=PRODUCT_RELATED_PRODUCT_CATEGORY('Belt guard','Belt guard',(#27687));
#27609=PRODUCT_RELATED_PRODUCT_CATEGORY(
'Sealed Ball Bearing - 10 x 30 x 9 mm',
'Sealed Ball Bearing - 10 x 30 x 9 mm',(#27688));
#27610=PRODUCT_RELATED_PRODUCT_CATEGORY('Inner ring','Inner ring',(#27689));
#27611=PRODUCT_RELATED_PRODUCT_CATEGORY('Outer ring','Outer ring',(#27690));
#27612=PRODUCT_RELATED_PRODUCT_CATEGORY('Balls','Balls',(#27691));
#27613=PRODUCT_RELATED_PRODUCT_CATEGORY('Cage','Cage',(#27692));
#27614=PRODUCT_RELATED_PRODUCT_CATEGORY('Seals 2RS','Seals 2RS',(#27693));
#27615=PRODUCT_RELATED_PRODUCT_CATEGORY('M4x30 mounting screw',
'M4x30 mounting screw',(#27694));
#27616=PRODUCT_RELATED_PRODUCT_CATEGORY(
'Sealed Ball Bearing - 12 x 32 x 10 mm',
'Sealed Ball Bearing - 12 x 32 x 10 mm',(#27695));
#27617=PRODUCT_RELATED_PRODUCT_CATEGORY('Inner ring (1)',
'Inner ring (1)',(#27696));
#27618=PRODUCT_RELATED_PRODUCT_CATEGORY('Outer ring (1)',
'Outer ring (1)',(#27697));
#27619=PRODUCT_RELATED_PRODUCT_CATEGORY('Balls (1)','Balls (1)',(#27698));
#27620=PRODUCT_RELATED_PRODUCT_CATEGORY('Cage (1)','Cage (1)',(#27699));
#27621=PRODUCT_RELATED_PRODUCT_CATEGORY('Seals 2RS (1)','Seals 2RS (1)',
(#27700));
#27622=PRODUCT_RELATED_PRODUCT_CATEGORY('Cap Screw - M5x20',
'Cap Screw - M5x20',(#27701));
#27623=PRODUCT_RELATED_PRODUCT_CATEGORY(
'Pillow Block Bearing - 20 mm Bore','Pillow Block Bearing - 20 mm Bore',
(#27702));
#27624=PRODUCT_RELATED_PRODUCT_CATEGORY('Housing','Housing',(#27703));
#27625=PRODUCT_RELATED_PRODUCT_CATEGORY('Insert bearing',
'Insert bearing',(#27704));
#27626=PRODUCT_RELATED_PRODUCT_CATEGORY('Flat Washer - M8',
'Flat Washer - M8',(#27705));
#27627=PRODUCT_RELATED_PRODUCT_CATEGORY('M8x25 Bolt','M8x25 Bolt',(#27706));
#27628=PRODUCT_RELATED_PRODUCT_CATEGORY('M4x10 Cap Screw',
'M4x10 Cap Screw',(#27707));
#27629=PRODUCT_RELATED_PRODUCT_CATEGORY('Input pulley and shaft',
'Input pulley and shaft',(#27708));
#27630=PRODUCT_RELATED_PRODUCT_CATEGORY('Input shaft','Input shaft',(#27709));
#27631=PRODUCT_RELATED_PRODUCT_CATEGORY('Input inner spacer',
'Input inner spacer',(#27710));
#27632=PRODUCT_RELATED_PRODUCT_CATEGORY('Input inner sleeve',
'Input inner sleeve',(#27711));
#27633=PRODUCT_RELATED_PRODUCT_CATEGORY('Input M3 set screw',
'Input M3 set screw',(#27712));
#27634=PRODUCT_RELATED_PRODUCT_CATEGORY('Input M3 set screw (1)',
'Input M3 set screw (1)',(#27713));
#27635=PRODUCT_RELATED_PRODUCT_CATEGORY('Input end keeper',
'Input end keeper',(#27714));
#27636=PRODUCT_RELATED_PRODUCT_CATEGORY('Motor output shaft',
'Motor output shaft',(#27715));
#27637=PRODUCT_RELATED_PRODUCT_CATEGORY('Motor coupling',
'Motor coupling',(#27716));
#27638=PRODUCT_RELATED_PRODUCT_CATEGORY(
'Timing Pulley - 2 mm Pitch, 20 Teeth, 8 mm Bore',
'Timing Pulley - 2 mm Pitch, 20 Teeth, 8 mm Bore',(#27717));
#27639=PRODUCT_RELATED_PRODUCT_CATEGORY('Output pulley and shaft',
'Output pulley and shaft',(#27718));
#27640=PRODUCT_RELATED_PRODUCT_CATEGORY('Output shaft','Output shaft',(#27719));
#27641=PRODUCT_RELATED_PRODUCT_CATEGORY('Output inner spacer',
'Output inner spacer',(#27720));
#27642=PRODUCT_RELATED_PRODUCT_CATEGORY('Output inner sleeve',
'Output inner sleeve',(#27721));
#27643=PRODUCT_RELATED_PRODUCT_CATEGORY('Output M3 set screw',
'Output M3 set screw',(#27722));
#27644=PRODUCT_RELATED_PRODUCT_CATEGORY('Output M3 set screw (1)',
'Output M3 set screw (1)',(#27723));
#27645=PRODUCT_RELATED_PRODUCT_CATEGORY('Output end keeper',
'Output end keeper',(#27724));
#27646=PRODUCT_RELATED_PRODUCT_CATEGORY('Drum shaft collar',
'Drum shaft collar',(#27725));
#27647=PRODUCT_RELATED_PRODUCT_CATEGORY('Drum shaft collar (1)',
'Drum shaft collar (1)',(#27726));
#27648=PRODUCT_RELATED_PRODUCT_CATEGORY('Conveyor drum shell',
'Conveyor drum shell',(#27727));
#27649=PRODUCT_RELATED_PRODUCT_CATEGORY('Drum end plate',
'Drum end plate',(#27728));
#27650=PRODUCT_RELATED_PRODUCT_CATEGORY('Drum end plate (1)',
'Drum end plate (1)',(#27729));
#27651=PRODUCT_RELATED_PRODUCT_CATEGORY('Drum hub','Drum hub',(#27730));
#27652=PRODUCT_RELATED_PRODUCT_CATEGORY('Drum hub (1)','Drum hub (1)',(#27731));
#27653=PRODUCT_RELATED_PRODUCT_CATEGORY(
'Timing Pulley - 2 mm Pitch, 40 Teeth, 12 mm Bore',
'Timing Pulley - 2 mm Pitch, 40 Teeth, 12 mm Bore',(#27732));
#27654=PRODUCT_RELATED_PRODUCT_CATEGORY('Cap Screw - M4x16',
'Cap Screw - M4x16',(#27733));
#27655=PRODUCT_RELATED_PRODUCT_CATEGORY('Socket Set Screw - M5x8',
'Socket Set Screw - M5x8',(#27734));
#27656=APPLICATION_PROTOCOL_DEFINITION('international standard',
'automotive_design',2009,#27657);
#27657=APPLICATION_CONTEXT(
'Core Data for Automotive Mechanical Design Process');
#27658=PRODUCT_CONTEXT('part definition',#27657,'mechanical');
#27659=PRODUCT('PAT-010','PAT-010',
'PAT-010',(#27658));
#27660=PRODUCT('Bearing base and belt envelope',
'Bearing base and belt envelope','Bearing base and belt envelope',(#27658));
#27661=PRODUCT('Base','Base','Base',(#27658));
#27662=PRODUCT('Foot','Foot','Foot',(#27658));
#27663=PRODUCT('Foot (1)','Foot (1)','Foot (1)',(#27658));
#27664=PRODUCT('Fixed bearing block','Fixed bearing block',
'Fixed bearing block',(#27658));
#27665=PRODUCT('Input outer spacer','Input outer spacer',
'Input outer spacer',(#27658));
#27666=PRODUCT('Input bearing cap','Input bearing cap',
'Input bearing cap',(#27658));
#27667=PRODUCT('Input bearing cap (1)','Input bearing cap (1)',
'Input bearing cap (1)',(#27658));
#27668=PRODUCT('Sliding bearing block','Sliding bearing block',
'Sliding bearing block',(#27658));
#27669=PRODUCT('M4 clamp nut','M4 clamp nut','M4 clamp nut',(#27658));
#27670=PRODUCT('M4 clamp nut (1)','M4 clamp nut (1)','M4 clamp nut (1)',(#27658));
#27671=PRODUCT('M4 clamp nut (2)','M4 clamp nut (2)','M4 clamp nut (2)',(#27658));
#27672=PRODUCT('M4 clamp nut (3)','M4 clamp nut (3)','M4 clamp nut (3)',(#27658));
#27673=PRODUCT('Output outer spacer','Output outer spacer',
'Output outer spacer',(#27658));
#27674=PRODUCT('Output bearing cap','Output bearing cap',
'Output bearing cap',(#27658));
#27675=PRODUCT('Output bearing cap (1)','Output bearing cap (1)',
'Output bearing cap (1)',(#27658));
#27676=PRODUCT('Timing belt backing envelope',
'Timing belt backing envelope','Timing belt backing envelope',(#27658));
#27677=PRODUCT('Drum bearing riser','Drum bearing riser',
'Drum bearing riser',(#27658));
#27678=PRODUCT('Bearing mounting bush','Bearing mounting bush',
'Bearing mounting bush',(#27658));
#27679=PRODUCT('Bearing mounting bush (1)','Bearing mounting bush (1)',
'Bearing mounting bush (1)',(#27658));
#27680=PRODUCT('Drum bearing riser (1)','Drum bearing riser (1)',
'Drum bearing riser (1)',(#27658));
#27681=PRODUCT('Bearing mounting bush (2)','Bearing mounting bush (2)',
'Bearing mounting bush (2)',(#27658));
#27682=PRODUCT('Bearing mounting bush (3)','Bearing mounting bush (3)',
'Bearing mounting bush (3)',(#27658));
#27683=PRODUCT('Motor pedestal','Motor pedestal','Motor pedestal',(#27658));
#27684=PRODUCT('Motor envelope','Motor envelope','Motor envelope',(#27658));
#27685=PRODUCT('Guard post','Guard post','Guard post',(#27658));
#27686=PRODUCT('Guard post (1)','Guard post (1)','Guard post (1)',(#27658));
#27687=PRODUCT('Belt guard','Belt guard','Belt guard',(#27658));
#27688=PRODUCT('Sealed Ball Bearing - 10 x 30 x 9 mm',
'Sealed Ball Bearing - 10 x 30 x 9 mm',
'Sealed Ball Bearing - 10 x 30 x 9 mm',(#27658));
#27689=PRODUCT('Inner ring','Inner ring','Inner ring',(#27658));
#27690=PRODUCT('Outer ring','Outer ring','Outer ring',(#27658));
#27691=PRODUCT('Balls','Balls','Balls',(#27658));
#27692=PRODUCT('Cage','Cage','Cage',(#27658));
#27693=PRODUCT('Seals 2RS','Seals 2RS','Seals 2RS',(#27658));
#27694=PRODUCT('M4x30 mounting screw','M4x30 mounting screw',
'M4x30 mounting screw',(#27658));
#27695=PRODUCT('Sealed Ball Bearing - 12 x 32 x 10 mm',
'Sealed Ball Bearing - 12 x 32 x 10 mm',
'Sealed Ball Bearing - 12 x 32 x 10 mm',(#27658));
#27696=PRODUCT('Inner ring (1)','Inner ring (1)','Inner ring (1)',(#27658));
#27697=PRODUCT('Outer ring (1)','Outer ring (1)','Outer ring (1)',(#27658));
#27698=PRODUCT('Balls (1)','Balls (1)','Balls (1)',(#27658));
#27699=PRODUCT('Cage (1)','Cage (1)','Cage (1)',(#27658));
#27700=PRODUCT('Seals 2RS (1)','Seals 2RS (1)','Seals 2RS (1)',(#27658));
#27701=PRODUCT('Cap Screw - M5x20','Cap Screw - M5x20',
'Cap Screw - M5x20',(#27658));
#27702=PRODUCT('Pillow Block Bearing - 20 mm Bore',
'Pillow Block Bearing - 20 mm Bore','Pillow Block Bearing - 20 mm Bore',
(#27658));
#27703=PRODUCT('Housing','Housing','Housing',(#27658));
#27704=PRODUCT('Insert bearing','Insert bearing','Insert bearing',(#27658));
#27705=PRODUCT('Flat Washer - M8','Flat Washer - M8','Flat Washer - M8',
(#27658));
#27706=PRODUCT('M8x25 Bolt','M8x25 Bolt','M8x25 Bolt',(#27658));
#27707=PRODUCT('M4x10 Cap Screw','M4x10 Cap Screw','M4x10 Cap Screw',(#27658));
#27708=PRODUCT('Input pulley and shaft','Input pulley and shaft',
'Input pulley and shaft',(#27658));
#27709=PRODUCT('Input shaft','Input shaft','Input shaft',(#27658));
#27710=PRODUCT('Input inner spacer','Input inner spacer',
'Input inner spacer',(#27658));
#27711=PRODUCT('Input inner sleeve','Input inner sleeve',
'Input inner sleeve',(#27658));
#27712=PRODUCT('Input M3 set screw','Input M3 set screw',
'Input M3 set screw',(#27658));
#27713=PRODUCT('Input M3 set screw (1)','Input M3 set screw (1)',
'Input M3 set screw (1)',(#27658));
#27714=PRODUCT('Input end keeper','Input end keeper','Input end keeper',
(#27658));
#27715=PRODUCT('Motor output shaft','Motor output shaft',
'Motor output shaft',(#27658));
#27716=PRODUCT('Motor coupling','Motor coupling','Motor coupling',(#27658));
#27717=PRODUCT('Timing Pulley - 2 mm Pitch, 20 Teeth, 8 mm Bore',
'Timing Pulley - 2 mm Pitch, 20 Teeth, 8 mm Bore',
'Timing Pulley - 2 mm Pitch, 20 Teeth, 8 mm Bore',(#27658));
#27718=PRODUCT('Output pulley and shaft','Output pulley and shaft',
'Output pulley and shaft',(#27658));
#27719=PRODUCT('Output shaft','Output shaft','Output shaft',(#27658));
#27720=PRODUCT('Output inner spacer','Output inner spacer',
'Output inner spacer',(#27658));
#27721=PRODUCT('Output inner sleeve','Output inner sleeve',
'Output inner sleeve',(#27658));
#27722=PRODUCT('Output M3 set screw','Output M3 set screw',
'Output M3 set screw',(#27658));
#27723=PRODUCT('Output M3 set screw (1)','Output M3 set screw (1)',
'Output M3 set screw (1)',(#27658));
#27724=PRODUCT('Output end keeper','Output end keeper',
'Output end keeper',(#27658));
#27725=PRODUCT('Drum shaft collar','Drum shaft collar',
'Drum shaft collar',(#27658));
#27726=PRODUCT('Drum shaft collar (1)','Drum shaft collar (1)',
'Drum shaft collar (1)',(#27658));
#27727=PRODUCT('Conveyor drum shell','Conveyor drum shell',
'Conveyor drum shell',(#27658));
#27728=PRODUCT('Drum end plate','Drum end plate','Drum end plate',(#27658));
#27729=PRODUCT('Drum end plate (1)','Drum end plate (1)','Drum end plate (1)',
(#27658));
#27730=PRODUCT('Drum hub','Drum hub','Drum hub',(#27658));
#27731=PRODUCT('Drum hub (1)','Drum hub (1)','Drum hub (1)',(#27658));
#27732=PRODUCT('Timing Pulley - 2 mm Pitch, 40 Teeth, 12 mm Bore',
'Timing Pulley - 2 mm Pitch, 40 Teeth, 12 mm Bore',
'Timing Pulley - 2 mm Pitch, 40 Teeth, 12 mm Bore',(#27658));
#27733=PRODUCT('Cap Screw - M4x16','Cap Screw - M4x16',
'Cap Screw - M4x16',(#27658));
#27734=PRODUCT('Socket Set Screw - M5x8','Socket Set Screw - M5x8',
'Socket Set Screw - M5x8',(#27658));
#27735=PRESENTATION_STYLE_ASSIGNMENT((#27740));
#27736=PRESENTATION_STYLE_ASSIGNMENT((#27741));
#27737=PRESENTATION_STYLE_ASSIGNMENT((#27742));
#27738=PRESENTATION_STYLE_ASSIGNMENT((#27743));
#27739=PRESENTATION_STYLE_ASSIGNMENT((#27744));
#27740=SURFACE_STYLE_USAGE(.BOTH.,#27745);
#27741=SURFACE_STYLE_USAGE(.BOTH.,#27746);
#27742=SURFACE_STYLE_USAGE(.BOTH.,#27747);
#27743=SURFACE_STYLE_USAGE(.BOTH.,#27748);
#27744=SURFACE_STYLE_USAGE(.BOTH.,#27749);
#27745=SURFACE_SIDE_STYLE('',(#27750));
#27746=SURFACE_SIDE_STYLE('',(#27751));
#27747=SURFACE_SIDE_STYLE('',(#27752));
#27748=SURFACE_SIDE_STYLE('',(#27753));
#27749=SURFACE_SIDE_STYLE('',(#27754));
#27750=SURFACE_STYLE_FILL_AREA(#27755);
#27751=SURFACE_STYLE_FILL_AREA(#27756);
#27752=SURFACE_STYLE_FILL_AREA(#27757);
#27753=SURFACE_STYLE_FILL_AREA(#27758);
#27754=SURFACE_STYLE_FILL_AREA(#27759);
#27755=FILL_AREA_STYLE('Steel - Satin',(#27760));
#27756=FILL_AREA_STYLE('CAD Library Painted - Deep blue',(#27761));
#27757=FILL_AREA_STYLE('CAD Library Painted - Steel gray',(#27762));
#27758=FILL_AREA_STYLE('CAD Library Painted - Engineering blue',(#27763));
#27759=FILL_AREA_STYLE('CAD Library Painted - Graphite',(#27764));
#27760=FILL_AREA_STYLE_COLOUR('Steel - Satin',#27765);
#27761=FILL_AREA_STYLE_COLOUR('CAD Library Painted - Deep blue',#27766);
#27762=FILL_AREA_STYLE_COLOUR('CAD Library Painted - Steel gray',#27767);
#27763=FILL_AREA_STYLE_COLOUR('CAD Library Painted - Engineering blue',
#27768);
#27764=FILL_AREA_STYLE_COLOUR('CAD Library Painted - Graphite',#27769);
#27765=COLOUR_RGB('Steel - Satin',0.627450980392157,0.627450980392157,0.627450980392157);
#27766=COLOUR_RGB('CAD Library Painted - Deep blue',0.0784313725490196,
0.203921568627451,0.349019607843137);
#27767=COLOUR_RGB('CAD Library Painted - Steel gray',0.592156862745098,
0.631372549019608,0.67843137254902);
#27768=COLOUR_RGB('CAD Library Painted - Engineering blue',0.12156862745098,
0.356862745098039,0.6);
#27769=COLOUR_RGB('CAD Library Painted - Graphite',0.168627450980392,0.192156862745098,
0.231372549019608);
#27770=COLOUR_RGB('Dark Blue',0.08,0.2,0.34);
#27771=FILL_AREA_STYLE_COLOUR('',#27770);
#27772=FILL_AREA_STYLE('',(#27771));
#27773=SURFACE_STYLE_FILL_AREA(#27772);
#27774=SURFACE_SIDE_STYLE('',(#27773));
#27775=SURFACE_STYLE_USAGE(.BOTH.,#27774);
#27776=PRESENTATION_STYLE_ASSIGNMENT((#27775));
#27777=COLOUR_RGB('Light Blue',0.38,0.62,0.78);
#27778=FILL_AREA_STYLE_COLOUR('',#27777);
#27779=FILL_AREA_STYLE('',(#27778));
#27780=SURFACE_STYLE_FILL_AREA(#27779);
#27781=SURFACE_SIDE_STYLE('',(#27780));
#27782=SURFACE_STYLE_USAGE(.BOTH.,#27781);
#27783=PRESENTATION_STYLE_ASSIGNMENT((#27782));
#27784=COLOUR_RGB('Sky Blue',0.24,0.69,0.87);
#27785=FILL_AREA_STYLE_COLOUR('',#27784);
#27786=FILL_AREA_STYLE('',(#27785));
#27787=SURFACE_STYLE_FILL_AREA(#27786);
#27788=SURFACE_SIDE_STYLE('',(#27787));
#27789=SURFACE_STYLE_USAGE(.BOTH.,#27788);
#27790=PRESENTATION_STYLE_ASSIGNMENT((#27789));
#27791=COLOUR_RGB('Grey',0.48,0.52,0.57);
#27792=FILL_AREA_STYLE_COLOUR('',#27791);
#27793=FILL_AREA_STYLE('',(#27792));
#27794=SURFACE_STYLE_FILL_AREA(#27793);
#27795=SURFACE_SIDE_STYLE('',(#27794));
#27796=SURFACE_STYLE_USAGE(.BOTH.,#27795);
#27797=PRESENTATION_STYLE_ASSIGNMENT((#27796));
#27798=COLOUR_RGB('Black',0.12,0.14,0.17);
#27799=FILL_AREA_STYLE_COLOUR('',#27798);
#27800=FILL_AREA_STYLE('',(#27799));
#27801=SURFACE_STYLE_FILL_AREA(#27800);
#27802=SURFACE_SIDE_STYLE('',(#27801));
#27803=SURFACE_STYLE_USAGE(.BOTH.,#27802);
#27804=PRESENTATION_STYLE_ASSIGNMENT((#27803));
#27805=COLOUR_RGB('Off White',0.89,0.88,0.83);
#27806=FILL_AREA_STYLE_COLOUR('',#27805);
#27807=FILL_AREA_STYLE('',(#27806));
#27808=SURFACE_STYLE_FILL_AREA(#27807);
#27809=SURFACE_SIDE_STYLE('',(#27808));
#27810=SURFACE_STYLE_USAGE(.BOTH.,#27809);
#27811=PRESENTATION_STYLE_ASSIGNMENT((#27810));
ENDSEC;
END-ISO-10303-21;
